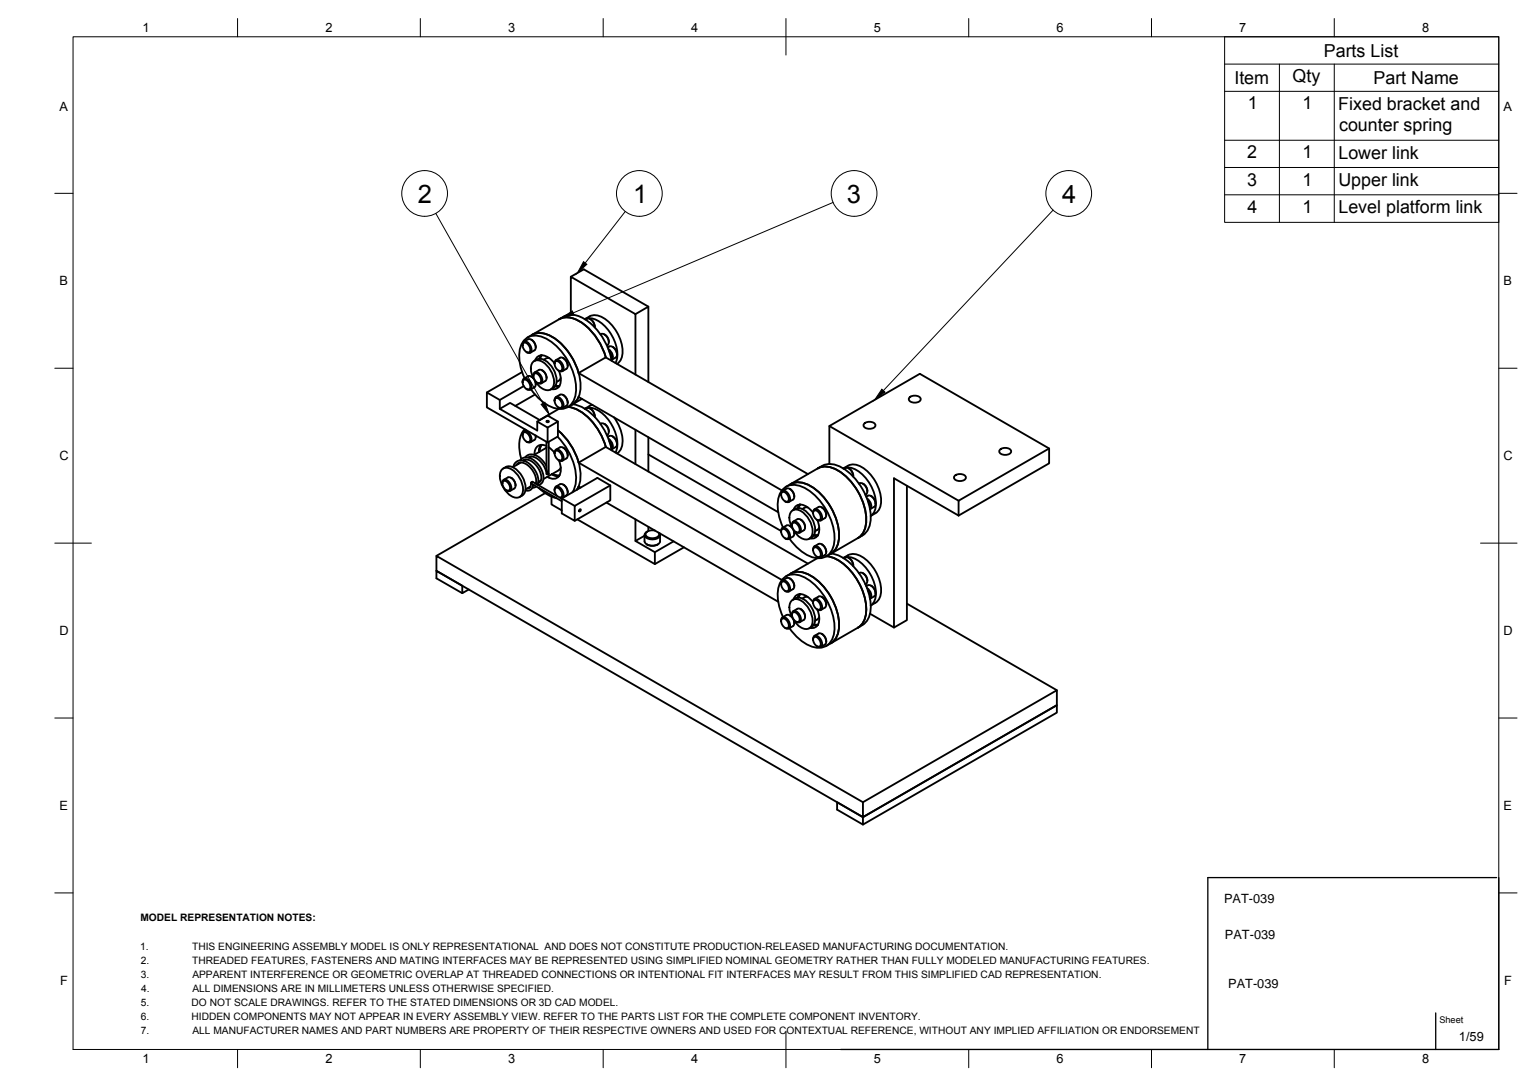
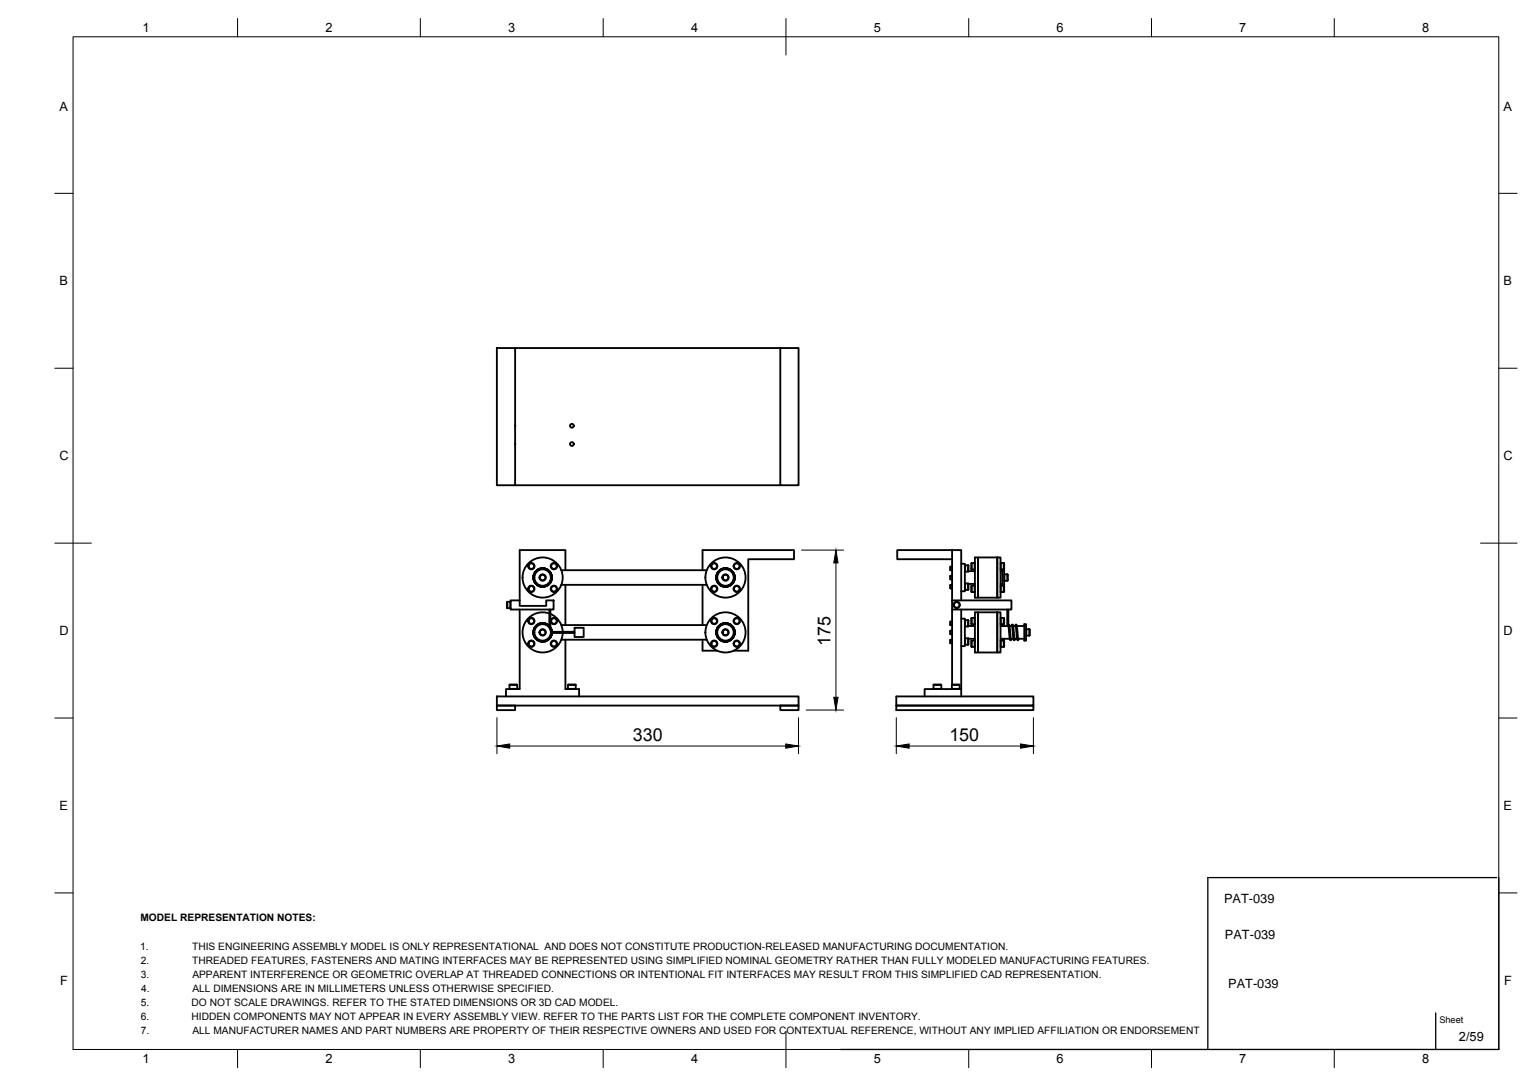
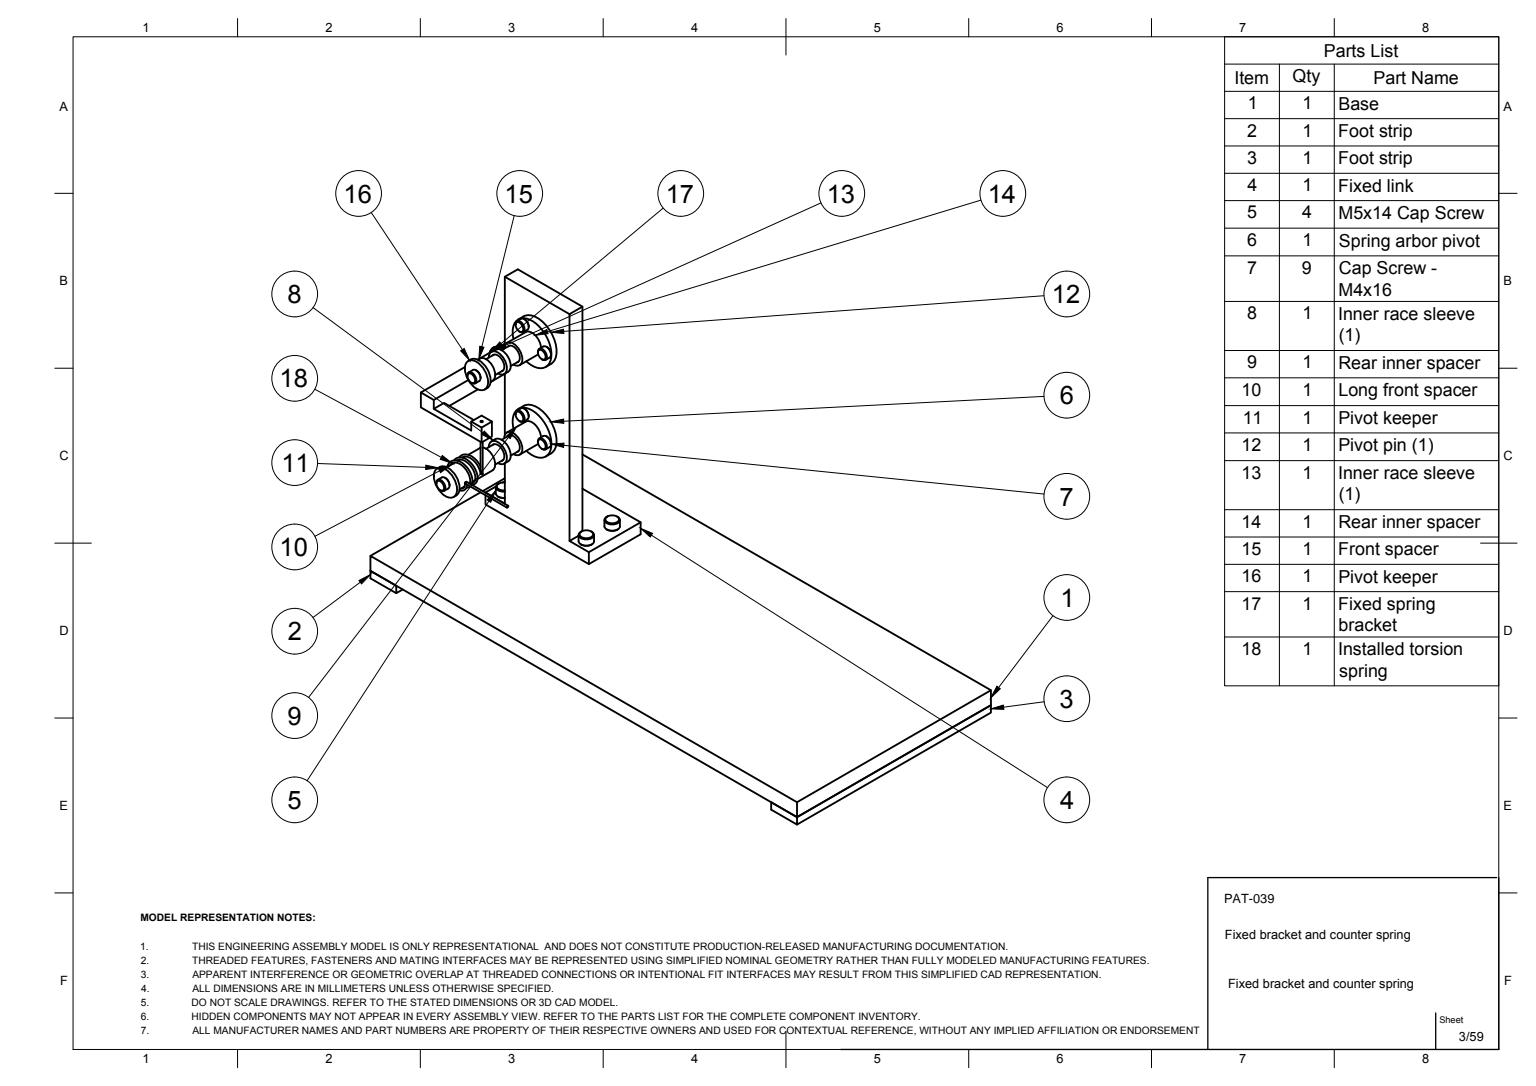
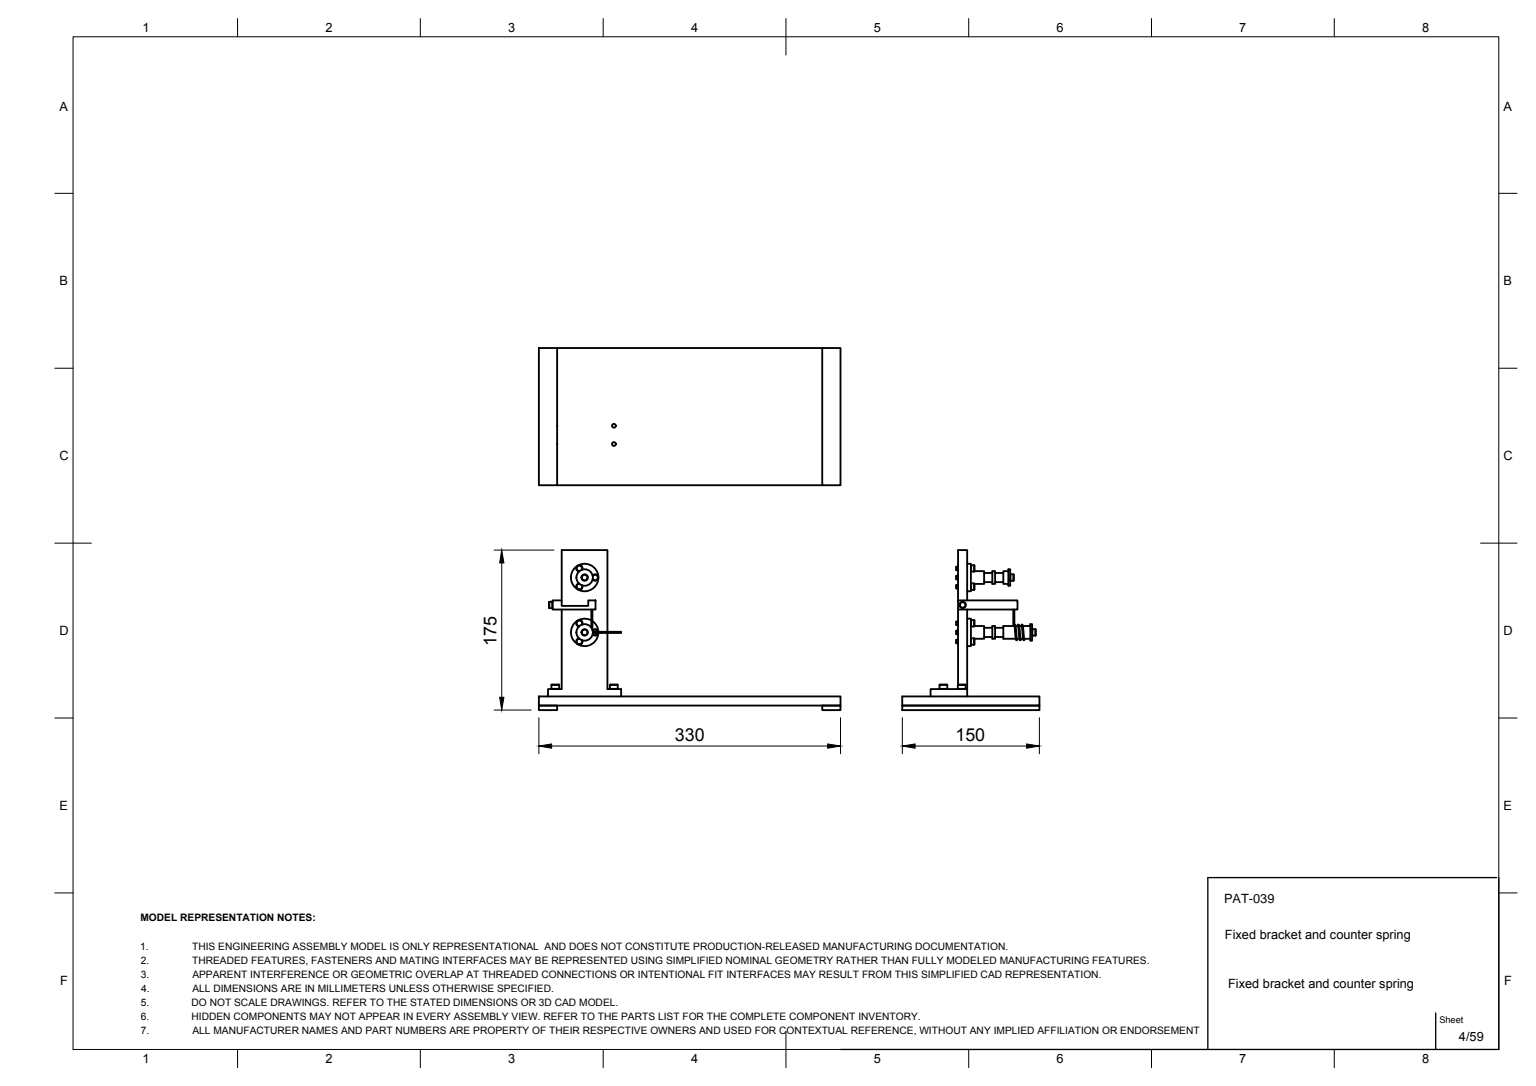
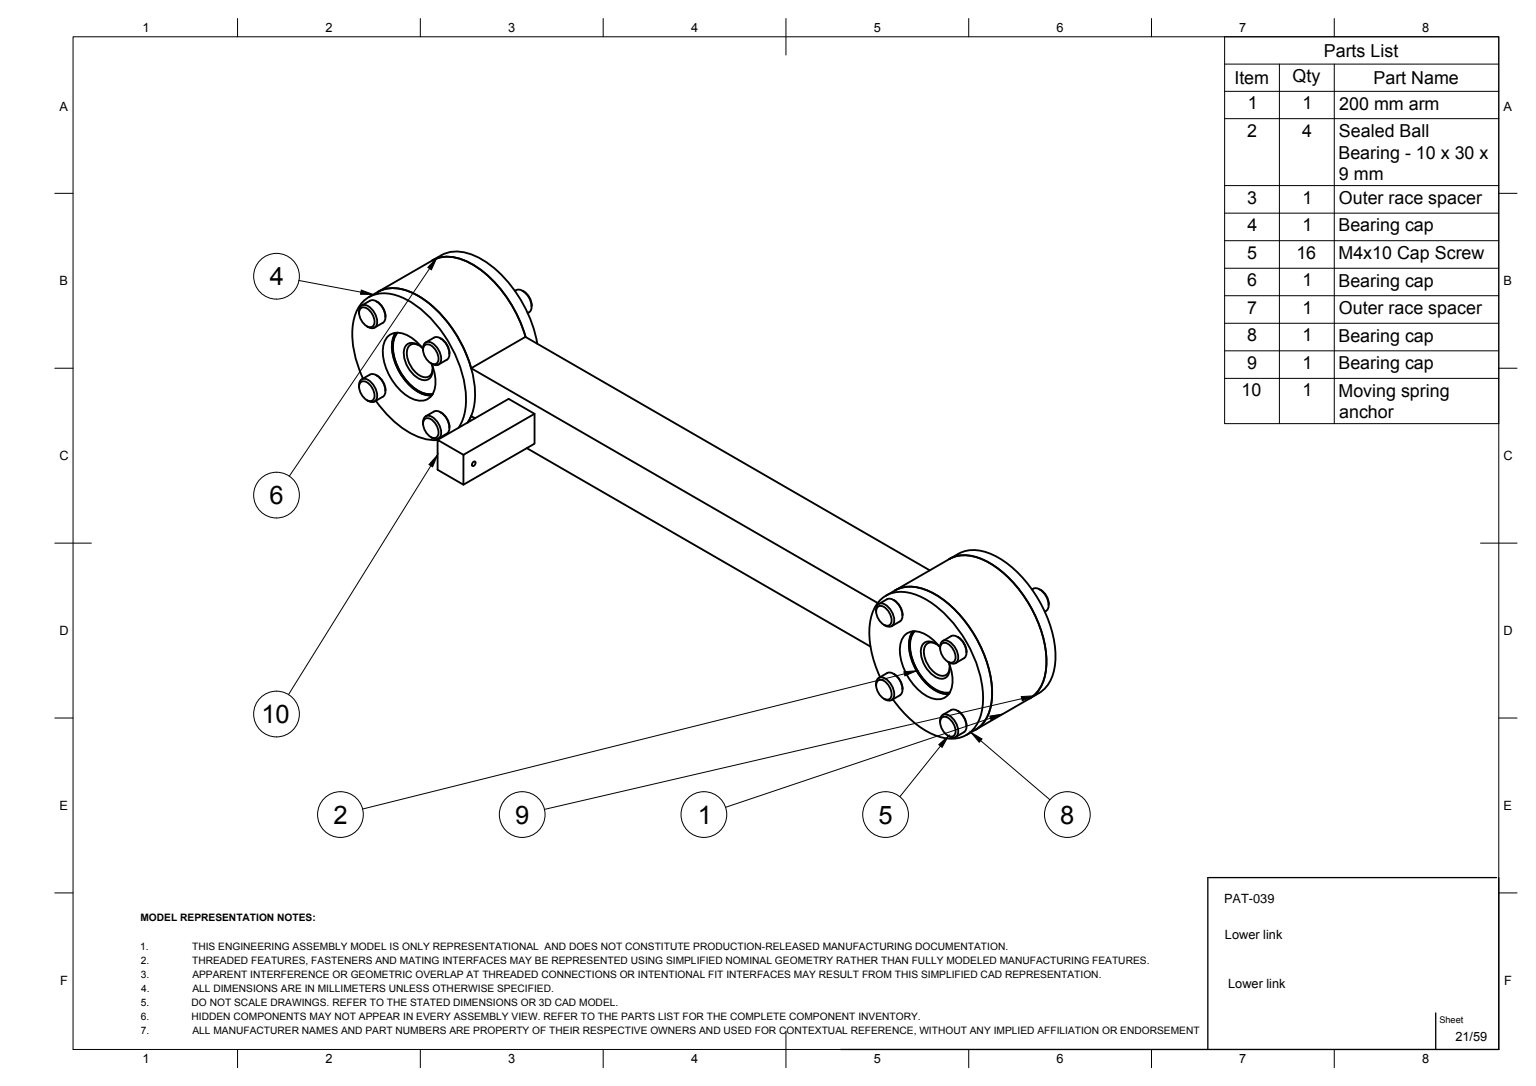
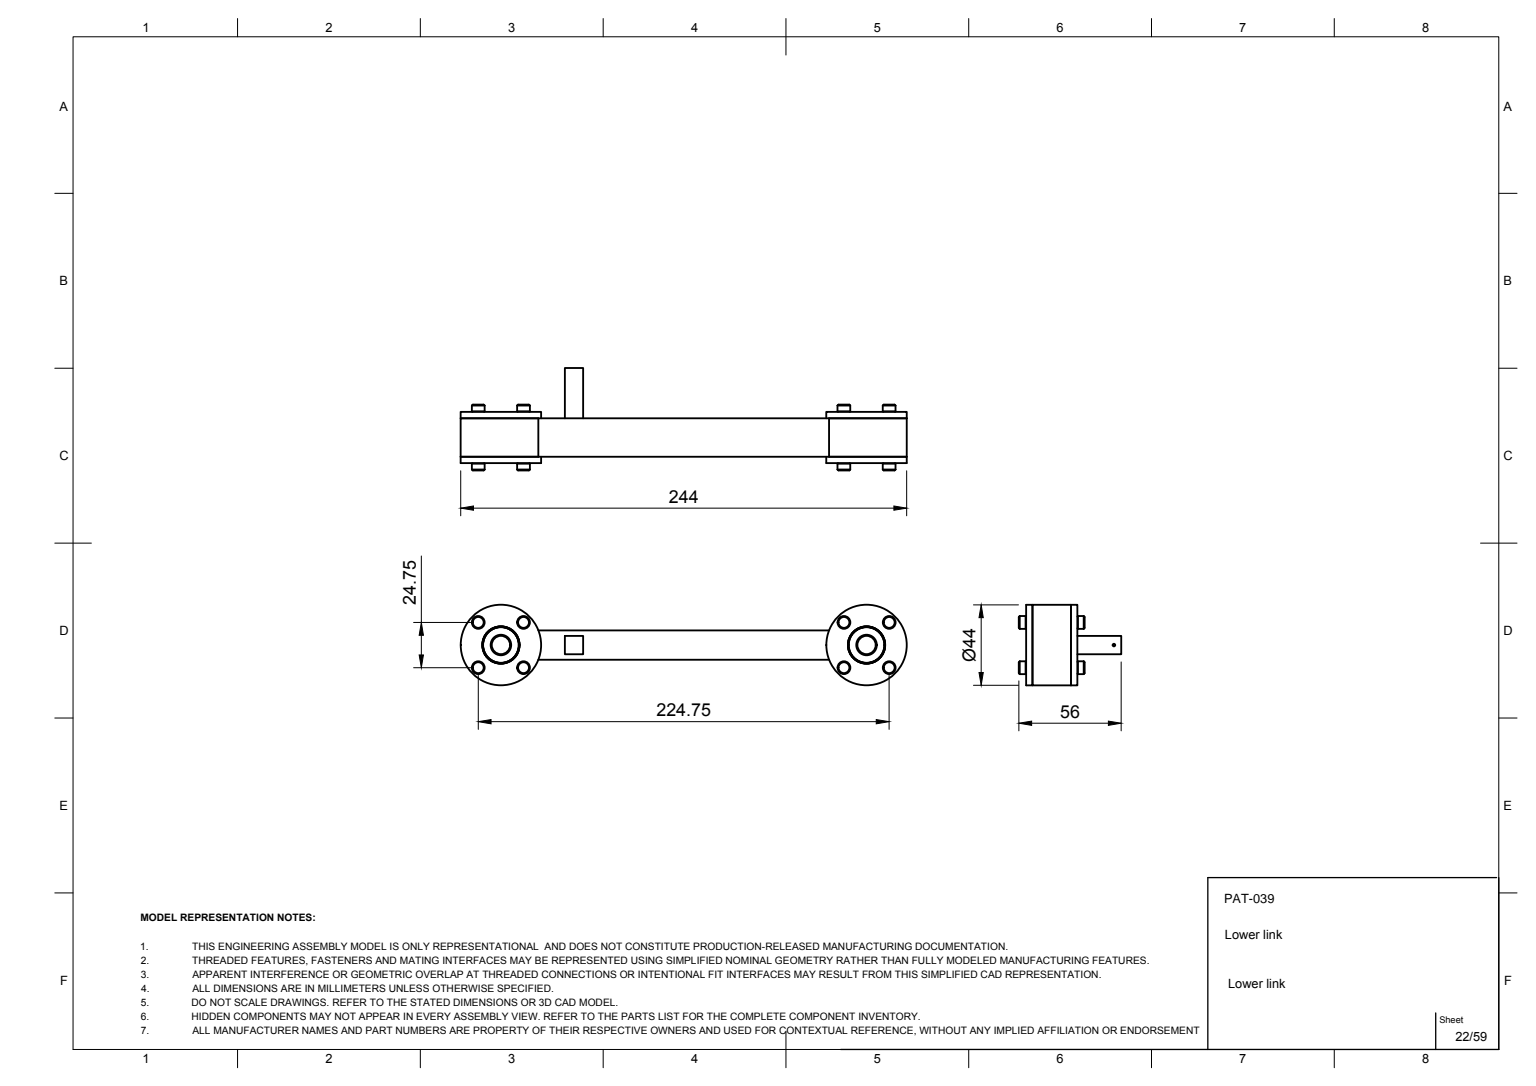
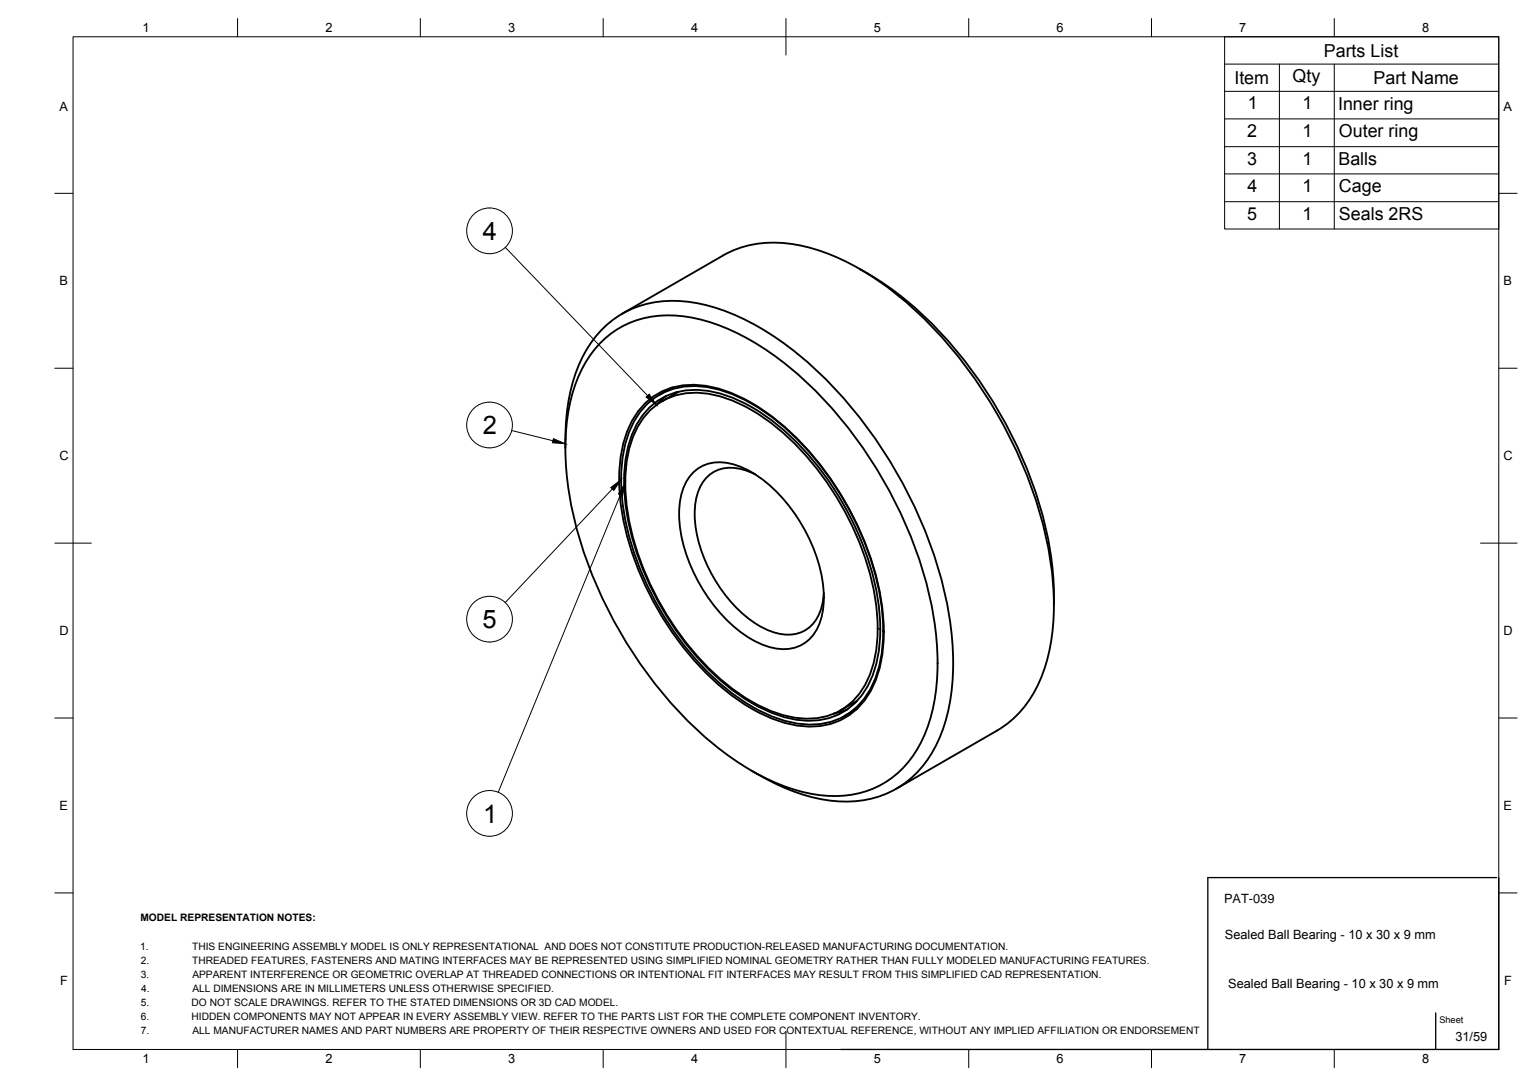
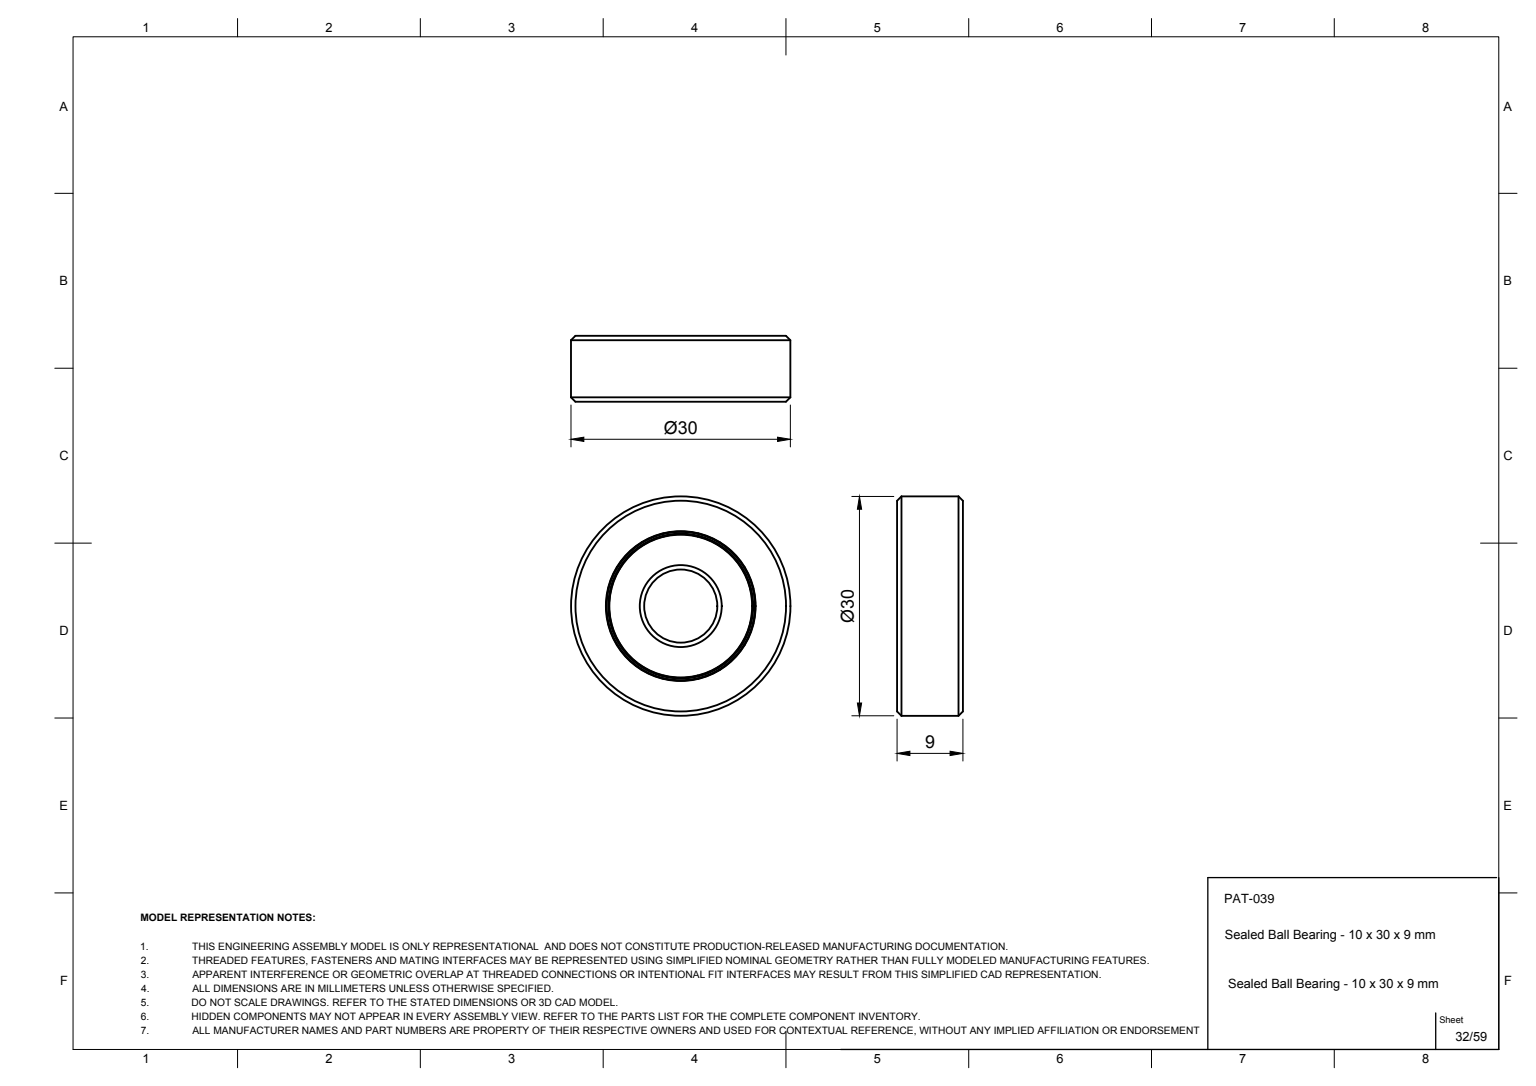
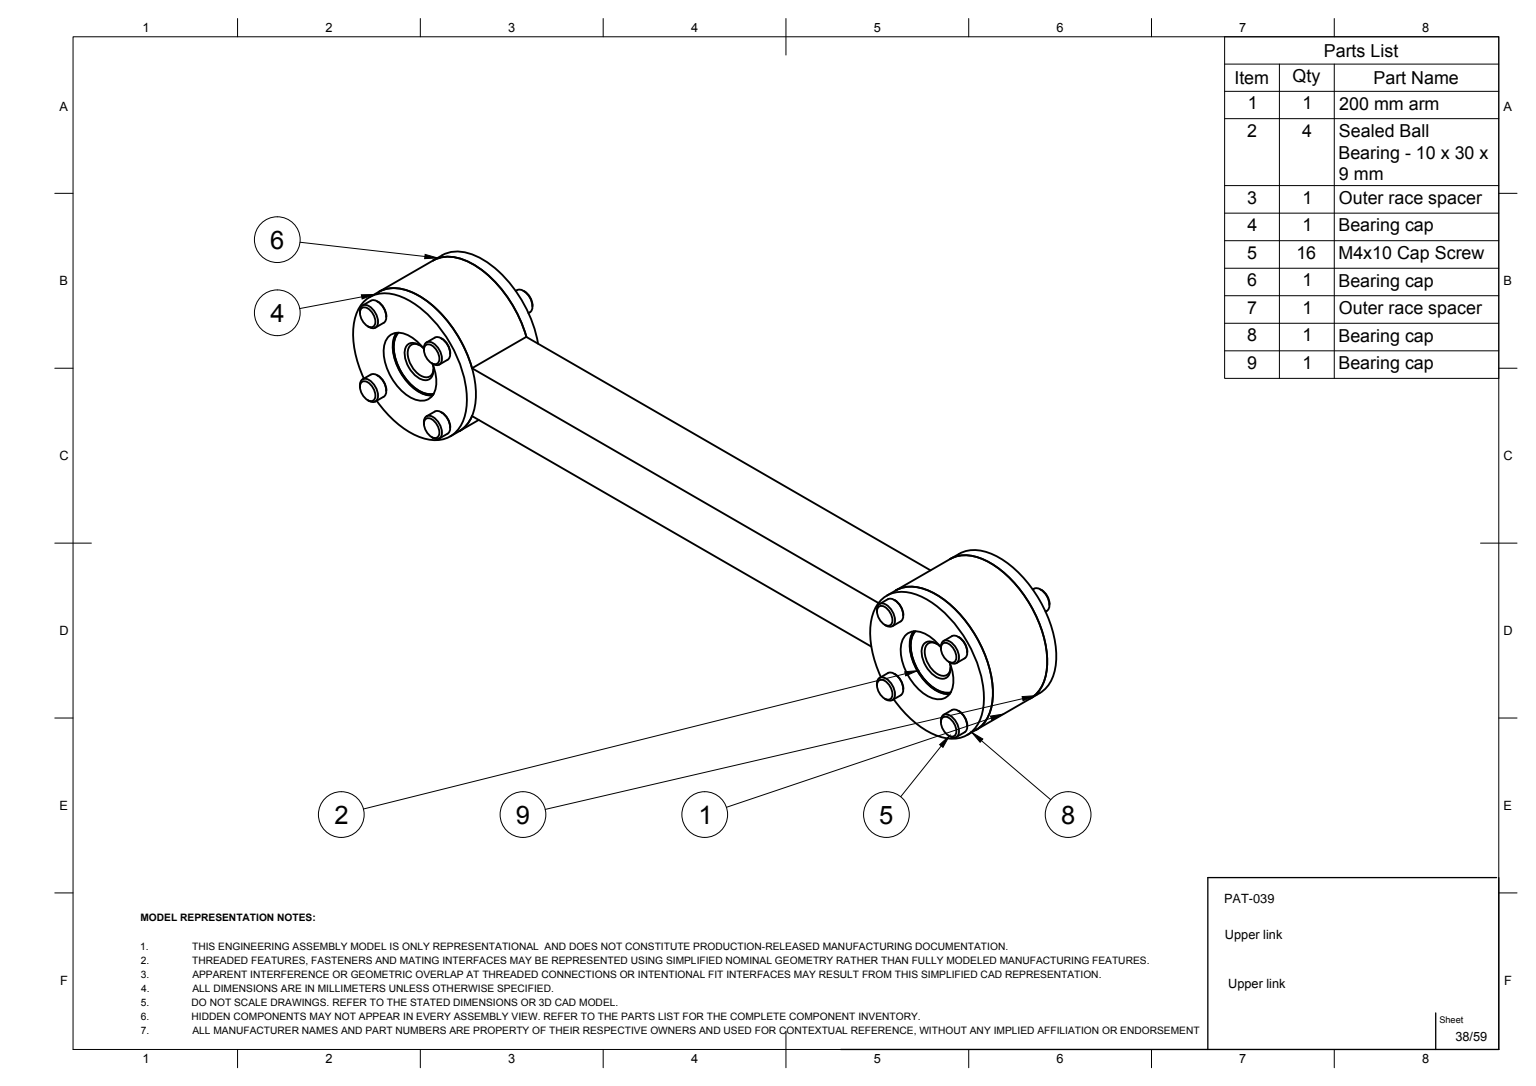
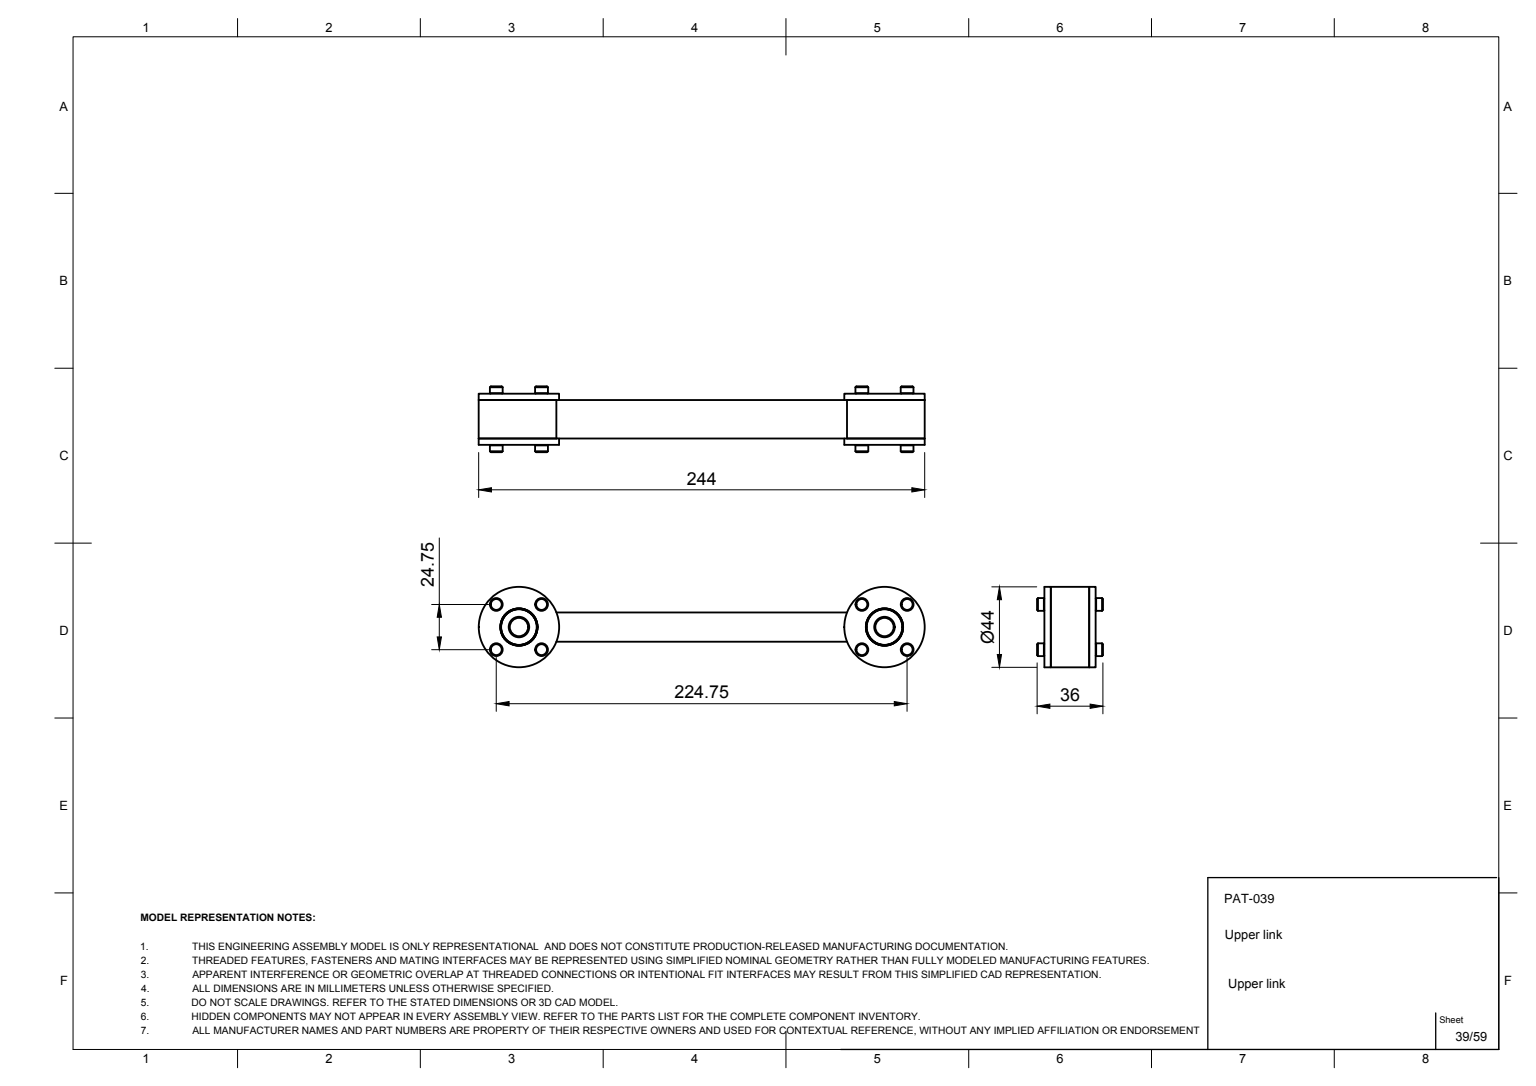
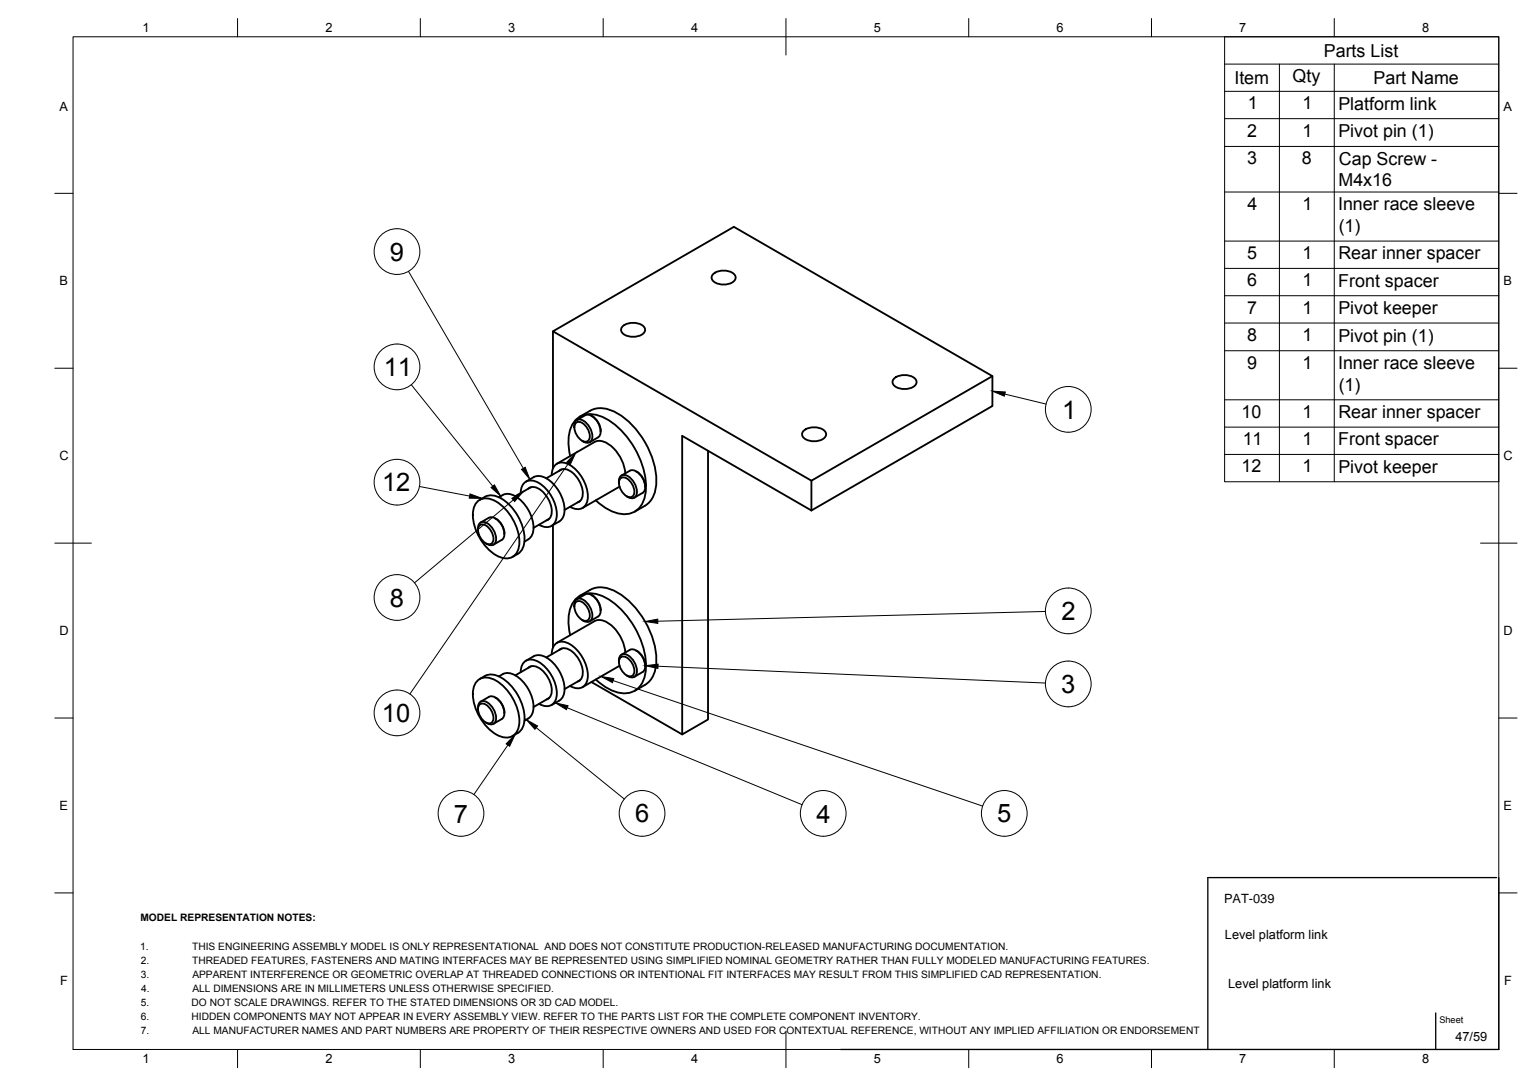
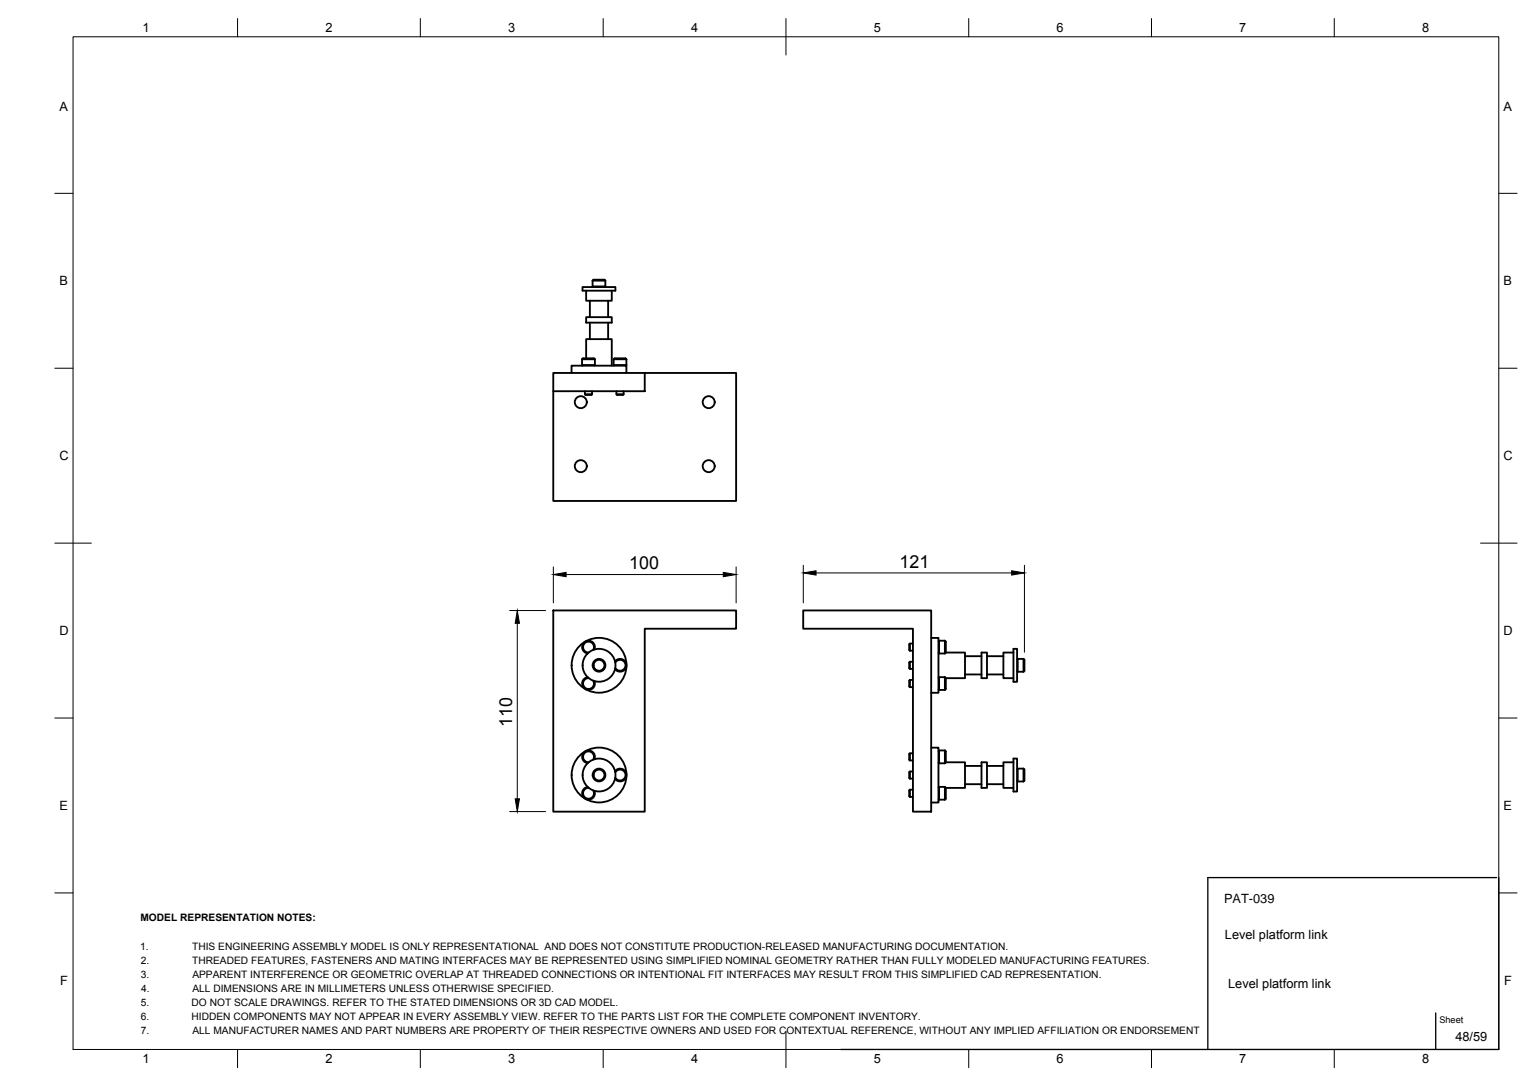
ISO-10303-21;
HEADER;
/* Generated by software containing ST-Developer
 * from STEP Tools, Inc. (www.steptools.com) 
 */

FILE_DESCRIPTION(
/* description */ ('Four-bar parallelogram arm'),
/* implementation_level */ '2;1');

FILE_NAME(
/* name */ 'PAT-039',
/* time_stamp */ '2026-10-28T03:24:55-07:00',
/* author */ (''),
/* organization */ (''),
/* preprocessor_version */ 'ST-DEVELOPER v20.2',
/* originating_system */ 'Autodesk Translation Framework v15.17.0.0',
/* authorisation */ '');

FILE_SCHEMA (('AUTOMOTIVE_DESIGN { 1 0 10303 214 3 1 1 }'));
ENDSEC;

DATA;
#10=MECHANICAL_DESIGN_GEOMETRIC_PRESENTATION_REPRESENTATION('',(#622,#623,
#624,#625,#626,#627,#628,#629,#630,#631,#632,#633,#634,#635,#636,#637,#638,
#639,#640,#641,#642,#643,#644,#645,#646,#647,#648,#649,#650,#651,#652,#653,
#654,#655,#656,#657,#658,#659,#660,#661,#662,#663,#664,#665,#666,#667,#668,
#669,#670,#671,#672,#673,#674,#675,#676,#677,#678,#679),#14512);
#11=ITEM_DEFINED_TRANSFORMATION($,$,#8507,#8635);
#12=ITEM_DEFINED_TRANSFORMATION($,$,#8527,#8636);
#13=ITEM_DEFINED_TRANSFORMATION($,$,#8547,#8637);
#14=ITEM_DEFINED_TRANSFORMATION($,$,#8564,#8638);
#15=ITEM_DEFINED_TRANSFORMATION($,$,#8618,#8639);
#16=ITEM_DEFINED_TRANSFORMATION($,$,#8209,#8664);
#17=ITEM_DEFINED_TRANSFORMATION($,$,#8250,#8665);
#18=ITEM_DEFINED_TRANSFORMATION($,$,#8259,#8666);
#19=ITEM_DEFINED_TRANSFORMATION($,$,#8280,#8667);
#20=ITEM_DEFINED_TRANSFORMATION($,$,#8301,#8668);
#21=ITEM_DEFINED_TRANSFORMATION($,$,#8310,#8669);
#22=ITEM_DEFINED_TRANSFORMATION($,$,#8331,#8670);
#23=ITEM_DEFINED_TRANSFORMATION($,$,#8352,#8671);
#24=ITEM_DEFINED_TRANSFORMATION($,$,#8506,#8672);
#25=ITEM_DEFINED_TRANSFORMATION($,$,#8506,#8673);
#26=ITEM_DEFINED_TRANSFORMATION($,$,#8640,#8674);
#27=ITEM_DEFINED_TRANSFORMATION($,$,#8640,#8675);
#28=ITEM_DEFINED_TRANSFORMATION($,$,#8640,#8676);
#29=ITEM_DEFINED_TRANSFORMATION($,$,#8640,#8677);
#30=ITEM_DEFINED_TRANSFORMATION($,$,#8640,#8678);
#31=ITEM_DEFINED_TRANSFORMATION($,$,#8640,#8679);
#32=ITEM_DEFINED_TRANSFORMATION($,$,#8640,#8680);
#33=ITEM_DEFINED_TRANSFORMATION($,$,#8640,#8681);
#34=ITEM_DEFINED_TRANSFORMATION($,$,#8506,#8682);
#35=ITEM_DEFINED_TRANSFORMATION($,$,#8506,#8683);
#36=ITEM_DEFINED_TRANSFORMATION($,$,#8640,#8684);
#37=ITEM_DEFINED_TRANSFORMATION($,$,#8640,#8685);
#38=ITEM_DEFINED_TRANSFORMATION($,$,#8640,#8686);
#39=ITEM_DEFINED_TRANSFORMATION($,$,#8640,#8687);
#40=ITEM_DEFINED_TRANSFORMATION($,$,#8640,#8688);
#41=ITEM_DEFINED_TRANSFORMATION($,$,#8640,#8689);
#42=ITEM_DEFINED_TRANSFORMATION($,$,#8640,#8690);
#43=ITEM_DEFINED_TRANSFORMATION($,$,#8640,#8691);
#44=ITEM_DEFINED_TRANSFORMATION($,$,#8363,#8692);
#45=ITEM_DEFINED_TRANSFORMATION($,$,#8404,#8693);
#46=ITEM_DEFINED_TRANSFORMATION($,$,#8413,#8694);
#47=ITEM_DEFINED_TRANSFORMATION($,$,#8434,#8695);
#48=ITEM_DEFINED_TRANSFORMATION($,$,#8455,#8696);
#49=ITEM_DEFINED_TRANSFORMATION($,$,#8464,#8697);
#50=ITEM_DEFINED_TRANSFORMATION($,$,#8485,#8698);
#51=ITEM_DEFINED_TRANSFORMATION($,$,#8506,#8699);
#52=ITEM_DEFINED_TRANSFORMATION($,$,#8506,#8700);
#53=ITEM_DEFINED_TRANSFORMATION($,$,#8640,#8701);
#54=ITEM_DEFINED_TRANSFORMATION($,$,#8640,#8702);
#55=ITEM_DEFINED_TRANSFORMATION($,$,#8640,#8703);
#56=ITEM_DEFINED_TRANSFORMATION($,$,#8640,#8704);
#57=ITEM_DEFINED_TRANSFORMATION($,$,#8640,#8705);
#58=ITEM_DEFINED_TRANSFORMATION($,$,#8640,#8706);
#59=ITEM_DEFINED_TRANSFORMATION($,$,#8640,#8707);
#60=ITEM_DEFINED_TRANSFORMATION($,$,#8640,#8708);
#61=ITEM_DEFINED_TRANSFORMATION($,$,#8506,#8709);
#62=ITEM_DEFINED_TRANSFORMATION($,$,#8506,#8710);
#63=ITEM_DEFINED_TRANSFORMATION($,$,#8640,#8711);
#64=ITEM_DEFINED_TRANSFORMATION($,$,#8640,#8712);
#65=ITEM_DEFINED_TRANSFORMATION($,$,#8640,#8713);
#66=ITEM_DEFINED_TRANSFORMATION($,$,#8640,#8714);
#67=ITEM_DEFINED_TRANSFORMATION($,$,#8640,#8715);
#68=ITEM_DEFINED_TRANSFORMATION($,$,#8640,#8716);
#69=ITEM_DEFINED_TRANSFORMATION($,$,#8640,#8717);
#70=ITEM_DEFINED_TRANSFORMATION($,$,#8640,#8718);
#71=ITEM_DEFINED_TRANSFORMATION($,$,#7940,#8918);
#72=ITEM_DEFINED_TRANSFORMATION($,$,#7959,#8919);
#73=ITEM_DEFINED_TRANSFORMATION($,$,#7966,#8920);
#74=ITEM_DEFINED_TRANSFORMATION($,$,#7973,#8921);
#75=ITEM_DEFINED_TRANSFORMATION($,$,#8024,#8922);
#76=ITEM_DEFINED_TRANSFORMATION($,$,#8051,#8923);
#77=ITEM_DEFINED_TRANSFORMATION($,$,#8060,#8924);
#78=ITEM_DEFINED_TRANSFORMATION($,$,#8069,#8925);
#79=ITEM_DEFINED_TRANSFORMATION($,$,#8078,#8926);
#80=ITEM_DEFINED_TRANSFORMATION($,$,#8087,#8927);
#81=ITEM_DEFINED_TRANSFORMATION($,$,#8114,#8928);
#82=ITEM_DEFINED_TRANSFORMATION($,$,#8123,#8929);
#83=ITEM_DEFINED_TRANSFORMATION($,$,#8132,#8930);
#84=ITEM_DEFINED_TRANSFORMATION($,$,#8141,#8931);
#85=ITEM_DEFINED_TRANSFORMATION($,$,#8150,#8932);
#86=ITEM_DEFINED_TRANSFORMATION($,$,#8168,#8933);
#87=ITEM_DEFINED_TRANSFORMATION($,$,#8184,#8934);
#88=ITEM_DEFINED_TRANSFORMATION($,$,#8184,#8935);
#89=ITEM_DEFINED_TRANSFORMATION($,$,#8184,#8936);
#90=ITEM_DEFINED_TRANSFORMATION($,$,#8184,#8937);
#91=ITEM_DEFINED_TRANSFORMATION($,$,#8892,#8938);
#92=ITEM_DEFINED_TRANSFORMATION($,$,#8892,#8939);
#93=ITEM_DEFINED_TRANSFORMATION($,$,#8892,#8940);
#94=ITEM_DEFINED_TRANSFORMATION($,$,#8892,#8941);
#95=ITEM_DEFINED_TRANSFORMATION($,$,#8892,#8942);
#96=ITEM_DEFINED_TRANSFORMATION($,$,#8892,#8943);
#97=ITEM_DEFINED_TRANSFORMATION($,$,#8892,#8944);
#98=ITEM_DEFINED_TRANSFORMATION($,$,#8892,#8945);
#99=ITEM_DEFINED_TRANSFORMATION($,$,#8892,#8946);
#100=ITEM_DEFINED_TRANSFORMATION($,$,#8720,#8947);
#101=ITEM_DEFINED_TRANSFORMATION($,$,#8766,#8948);
#102=ITEM_DEFINED_TRANSFORMATION($,$,#8793,#8949);
#103=ITEM_DEFINED_TRANSFORMATION($,$,#8802,#8950);
#104=ITEM_DEFINED_TRANSFORMATION($,$,#8811,#8951);
#105=ITEM_DEFINED_TRANSFORMATION($,$,#8820,#8952);
#106=ITEM_DEFINED_TRANSFORMATION($,$,#8829,#8953);
#107=ITEM_DEFINED_TRANSFORMATION($,$,#8856,#8954);
#108=ITEM_DEFINED_TRANSFORMATION($,$,#8865,#8955);
#109=ITEM_DEFINED_TRANSFORMATION($,$,#8874,#8956);
#110=ITEM_DEFINED_TRANSFORMATION($,$,#8883,#8957);
#111=ITEM_DEFINED_TRANSFORMATION($,$,#8892,#8958);
#112=ITEM_DEFINED_TRANSFORMATION($,$,#8892,#8959);
#113=ITEM_DEFINED_TRANSFORMATION($,$,#8892,#8960);
#114=ITEM_DEFINED_TRANSFORMATION($,$,#8892,#8961);
#115=ITEM_DEFINED_TRANSFORMATION($,$,#8892,#8962);
#116=ITEM_DEFINED_TRANSFORMATION($,$,#8892,#8963);
#117=ITEM_DEFINED_TRANSFORMATION($,$,#8892,#8964);
#118=ITEM_DEFINED_TRANSFORMATION($,$,#8892,#8965);
#119=ITEM_DEFINED_TRANSFORMATION($,$,#7939,#8966);
#120=ITEM_DEFINED_TRANSFORMATION($,$,#8208,#8967);
#121=ITEM_DEFINED_TRANSFORMATION($,$,#8362,#8968);
#122=ITEM_DEFINED_TRANSFORMATION($,$,#8719,#8969);
#123=(
REPRESENTATION_RELATIONSHIP($,$,#14778,#14777)
REPRESENTATION_RELATIONSHIP_WITH_TRANSFORMATION(#11)
SHAPE_REPRESENTATION_RELATIONSHIP()
);
#124=(
REPRESENTATION_RELATIONSHIP($,$,#14779,#14777)
REPRESENTATION_RELATIONSHIP_WITH_TRANSFORMATION(#12)
SHAPE_REPRESENTATION_RELATIONSHIP()
);
#125=(
REPRESENTATION_RELATIONSHIP($,$,#14780,#14777)
REPRESENTATION_RELATIONSHIP_WITH_TRANSFORMATION(#13)
SHAPE_REPRESENTATION_RELATIONSHIP()
);
#126=(
REPRESENTATION_RELATIONSHIP($,$,#14781,#14777)
REPRESENTATION_RELATIONSHIP_WITH_TRANSFORMATION(#14)
SHAPE_REPRESENTATION_RELATIONSHIP()
);
#127=(
REPRESENTATION_RELATIONSHIP($,$,#14782,#14777)
REPRESENTATION_RELATIONSHIP_WITH_TRANSFORMATION(#15)
SHAPE_REPRESENTATION_RELATIONSHIP()
);
#128=(
REPRESENTATION_RELATIONSHIP($,$,#14761,#14760)
REPRESENTATION_RELATIONSHIP_WITH_TRANSFORMATION(#16)
SHAPE_REPRESENTATION_RELATIONSHIP()
);
#129=(
REPRESENTATION_RELATIONSHIP($,$,#14762,#14760)
REPRESENTATION_RELATIONSHIP_WITH_TRANSFORMATION(#17)
SHAPE_REPRESENTATION_RELATIONSHIP()
);
#130=(
REPRESENTATION_RELATIONSHIP($,$,#14763,#14760)
REPRESENTATION_RELATIONSHIP_WITH_TRANSFORMATION(#18)
SHAPE_REPRESENTATION_RELATIONSHIP()
);
#131=(
REPRESENTATION_RELATIONSHIP($,$,#14764,#14760)
REPRESENTATION_RELATIONSHIP_WITH_TRANSFORMATION(#19)
SHAPE_REPRESENTATION_RELATIONSHIP()
);
#132=(
REPRESENTATION_RELATIONSHIP($,$,#14765,#14760)
REPRESENTATION_RELATIONSHIP_WITH_TRANSFORMATION(#20)
SHAPE_REPRESENTATION_RELATIONSHIP()
);
#133=(
REPRESENTATION_RELATIONSHIP($,$,#14766,#14760)
REPRESENTATION_RELATIONSHIP_WITH_TRANSFORMATION(#21)
SHAPE_REPRESENTATION_RELATIONSHIP()
);
#134=(
REPRESENTATION_RELATIONSHIP($,$,#14767,#14760)
REPRESENTATION_RELATIONSHIP_WITH_TRANSFORMATION(#22)
SHAPE_REPRESENTATION_RELATIONSHIP()
);
#135=(
REPRESENTATION_RELATIONSHIP($,$,#14768,#14760)
REPRESENTATION_RELATIONSHIP_WITH_TRANSFORMATION(#23)
SHAPE_REPRESENTATION_RELATIONSHIP()
);
#136=(
REPRESENTATION_RELATIONSHIP($,$,#14777,#14760)
REPRESENTATION_RELATIONSHIP_WITH_TRANSFORMATION(#24)
SHAPE_REPRESENTATION_RELATIONSHIP()
);
#137=(
REPRESENTATION_RELATIONSHIP($,$,#14777,#14760)
REPRESENTATION_RELATIONSHIP_WITH_TRANSFORMATION(#25)
SHAPE_REPRESENTATION_RELATIONSHIP()
);
#138=(
REPRESENTATION_RELATIONSHIP($,$,#14783,#14760)
REPRESENTATION_RELATIONSHIP_WITH_TRANSFORMATION(#26)
SHAPE_REPRESENTATION_RELATIONSHIP()
);
#139=(
REPRESENTATION_RELATIONSHIP($,$,#14783,#14760)
REPRESENTATION_RELATIONSHIP_WITH_TRANSFORMATION(#27)
SHAPE_REPRESENTATION_RELATIONSHIP()
);
#140=(
REPRESENTATION_RELATIONSHIP($,$,#14783,#14760)
REPRESENTATION_RELATIONSHIP_WITH_TRANSFORMATION(#28)
SHAPE_REPRESENTATION_RELATIONSHIP()
);
#141=(
REPRESENTATION_RELATIONSHIP($,$,#14783,#14760)
REPRESENTATION_RELATIONSHIP_WITH_TRANSFORMATION(#29)
SHAPE_REPRESENTATION_RELATIONSHIP()
);
#142=(
REPRESENTATION_RELATIONSHIP($,$,#14783,#14760)
REPRESENTATION_RELATIONSHIP_WITH_TRANSFORMATION(#30)
SHAPE_REPRESENTATION_RELATIONSHIP()
);
#143=(
REPRESENTATION_RELATIONSHIP($,$,#14783,#14760)
REPRESENTATION_RELATIONSHIP_WITH_TRANSFORMATION(#31)
SHAPE_REPRESENTATION_RELATIONSHIP()
);
#144=(
REPRESENTATION_RELATIONSHIP($,$,#14783,#14760)
REPRESENTATION_RELATIONSHIP_WITH_TRANSFORMATION(#32)
SHAPE_REPRESENTATION_RELATIONSHIP()
);
#145=(
REPRESENTATION_RELATIONSHIP($,$,#14783,#14760)
REPRESENTATION_RELATIONSHIP_WITH_TRANSFORMATION(#33)
SHAPE_REPRESENTATION_RELATIONSHIP()
);
#146=(
REPRESENTATION_RELATIONSHIP($,$,#14777,#14760)
REPRESENTATION_RELATIONSHIP_WITH_TRANSFORMATION(#34)
SHAPE_REPRESENTATION_RELATIONSHIP()
);
#147=(
REPRESENTATION_RELATIONSHIP($,$,#14777,#14760)
REPRESENTATION_RELATIONSHIP_WITH_TRANSFORMATION(#35)
SHAPE_REPRESENTATION_RELATIONSHIP()
);
#148=(
REPRESENTATION_RELATIONSHIP($,$,#14783,#14760)
REPRESENTATION_RELATIONSHIP_WITH_TRANSFORMATION(#36)
SHAPE_REPRESENTATION_RELATIONSHIP()
);
#149=(
REPRESENTATION_RELATIONSHIP($,$,#14783,#14760)
REPRESENTATION_RELATIONSHIP_WITH_TRANSFORMATION(#37)
SHAPE_REPRESENTATION_RELATIONSHIP()
);
#150=(
REPRESENTATION_RELATIONSHIP($,$,#14783,#14760)
REPRESENTATION_RELATIONSHIP_WITH_TRANSFORMATION(#38)
SHAPE_REPRESENTATION_RELATIONSHIP()
);
#151=(
REPRESENTATION_RELATIONSHIP($,$,#14783,#14760)
REPRESENTATION_RELATIONSHIP_WITH_TRANSFORMATION(#39)
SHAPE_REPRESENTATION_RELATIONSHIP()
);
#152=(
REPRESENTATION_RELATIONSHIP($,$,#14783,#14760)
REPRESENTATION_RELATIONSHIP_WITH_TRANSFORMATION(#40)
SHAPE_REPRESENTATION_RELATIONSHIP()
);
#153=(
REPRESENTATION_RELATIONSHIP($,$,#14783,#14760)
REPRESENTATION_RELATIONSHIP_WITH_TRANSFORMATION(#41)
SHAPE_REPRESENTATION_RELATIONSHIP()
);
#154=(
REPRESENTATION_RELATIONSHIP($,$,#14783,#14760)
REPRESENTATION_RELATIONSHIP_WITH_TRANSFORMATION(#42)
SHAPE_REPRESENTATION_RELATIONSHIP()
);
#155=(
REPRESENTATION_RELATIONSHIP($,$,#14783,#14760)
REPRESENTATION_RELATIONSHIP_WITH_TRANSFORMATION(#43)
SHAPE_REPRESENTATION_RELATIONSHIP()
);
#156=(
REPRESENTATION_RELATIONSHIP($,$,#14770,#14769)
REPRESENTATION_RELATIONSHIP_WITH_TRANSFORMATION(#44)
SHAPE_REPRESENTATION_RELATIONSHIP()
);
#157=(
REPRESENTATION_RELATIONSHIP($,$,#14771,#14769)
REPRESENTATION_RELATIONSHIP_WITH_TRANSFORMATION(#45)
SHAPE_REPRESENTATION_RELATIONSHIP()
);
#158=(
REPRESENTATION_RELATIONSHIP($,$,#14772,#14769)
REPRESENTATION_RELATIONSHIP_WITH_TRANSFORMATION(#46)
SHAPE_REPRESENTATION_RELATIONSHIP()
);
#159=(
REPRESENTATION_RELATIONSHIP($,$,#14773,#14769)
REPRESENTATION_RELATIONSHIP_WITH_TRANSFORMATION(#47)
SHAPE_REPRESENTATION_RELATIONSHIP()
);
#160=(
REPRESENTATION_RELATIONSHIP($,$,#14774,#14769)
REPRESENTATION_RELATIONSHIP_WITH_TRANSFORMATION(#48)
SHAPE_REPRESENTATION_RELATIONSHIP()
);
#161=(
REPRESENTATION_RELATIONSHIP($,$,#14775,#14769)
REPRESENTATION_RELATIONSHIP_WITH_TRANSFORMATION(#49)
SHAPE_REPRESENTATION_RELATIONSHIP()
);
#162=(
REPRESENTATION_RELATIONSHIP($,$,#14776,#14769)
REPRESENTATION_RELATIONSHIP_WITH_TRANSFORMATION(#50)
SHAPE_REPRESENTATION_RELATIONSHIP()
);
#163=(
REPRESENTATION_RELATIONSHIP($,$,#14777,#14769)
REPRESENTATION_RELATIONSHIP_WITH_TRANSFORMATION(#51)
SHAPE_REPRESENTATION_RELATIONSHIP()
);
#164=(
REPRESENTATION_RELATIONSHIP($,$,#14777,#14769)
REPRESENTATION_RELATIONSHIP_WITH_TRANSFORMATION(#52)
SHAPE_REPRESENTATION_RELATIONSHIP()
);
#165=(
REPRESENTATION_RELATIONSHIP($,$,#14783,#14769)
REPRESENTATION_RELATIONSHIP_WITH_TRANSFORMATION(#53)
SHAPE_REPRESENTATION_RELATIONSHIP()
);
#166=(
REPRESENTATION_RELATIONSHIP($,$,#14783,#14769)
REPRESENTATION_RELATIONSHIP_WITH_TRANSFORMATION(#54)
SHAPE_REPRESENTATION_RELATIONSHIP()
);
#167=(
REPRESENTATION_RELATIONSHIP($,$,#14783,#14769)
REPRESENTATION_RELATIONSHIP_WITH_TRANSFORMATION(#55)
SHAPE_REPRESENTATION_RELATIONSHIP()
);
#168=(
REPRESENTATION_RELATIONSHIP($,$,#14783,#14769)
REPRESENTATION_RELATIONSHIP_WITH_TRANSFORMATION(#56)
SHAPE_REPRESENTATION_RELATIONSHIP()
);
#169=(
REPRESENTATION_RELATIONSHIP($,$,#14783,#14769)
REPRESENTATION_RELATIONSHIP_WITH_TRANSFORMATION(#57)
SHAPE_REPRESENTATION_RELATIONSHIP()
);
#170=(
REPRESENTATION_RELATIONSHIP($,$,#14783,#14769)
REPRESENTATION_RELATIONSHIP_WITH_TRANSFORMATION(#58)
SHAPE_REPRESENTATION_RELATIONSHIP()
);
#171=(
REPRESENTATION_RELATIONSHIP($,$,#14783,#14769)
REPRESENTATION_RELATIONSHIP_WITH_TRANSFORMATION(#59)
SHAPE_REPRESENTATION_RELATIONSHIP()
);
#172=(
REPRESENTATION_RELATIONSHIP($,$,#14783,#14769)
REPRESENTATION_RELATIONSHIP_WITH_TRANSFORMATION(#60)
SHAPE_REPRESENTATION_RELATIONSHIP()
);
#173=(
REPRESENTATION_RELATIONSHIP($,$,#14777,#14769)
REPRESENTATION_RELATIONSHIP_WITH_TRANSFORMATION(#61)
SHAPE_REPRESENTATION_RELATIONSHIP()
);
#174=(
REPRESENTATION_RELATIONSHIP($,$,#14777,#14769)
REPRESENTATION_RELATIONSHIP_WITH_TRANSFORMATION(#62)
SHAPE_REPRESENTATION_RELATIONSHIP()
);
#175=(
REPRESENTATION_RELATIONSHIP($,$,#14783,#14769)
REPRESENTATION_RELATIONSHIP_WITH_TRANSFORMATION(#63)
SHAPE_REPRESENTATION_RELATIONSHIP()
);
#176=(
REPRESENTATION_RELATIONSHIP($,$,#14783,#14769)
REPRESENTATION_RELATIONSHIP_WITH_TRANSFORMATION(#64)
SHAPE_REPRESENTATION_RELATIONSHIP()
);
#177=(
REPRESENTATION_RELATIONSHIP($,$,#14783,#14769)
REPRESENTATION_RELATIONSHIP_WITH_TRANSFORMATION(#65)
SHAPE_REPRESENTATION_RELATIONSHIP()
);
#178=(
REPRESENTATION_RELATIONSHIP($,$,#14783,#14769)
REPRESENTATION_RELATIONSHIP_WITH_TRANSFORMATION(#66)
SHAPE_REPRESENTATION_RELATIONSHIP()
);
#179=(
REPRESENTATION_RELATIONSHIP($,$,#14783,#14769)
REPRESENTATION_RELATIONSHIP_WITH_TRANSFORMATION(#67)
SHAPE_REPRESENTATION_RELATIONSHIP()
);
#180=(
REPRESENTATION_RELATIONSHIP($,$,#14783,#14769)
REPRESENTATION_RELATIONSHIP_WITH_TRANSFORMATION(#68)
SHAPE_REPRESENTATION_RELATIONSHIP()
);
#181=(
REPRESENTATION_RELATIONSHIP($,$,#14783,#14769)
REPRESENTATION_RELATIONSHIP_WITH_TRANSFORMATION(#69)
SHAPE_REPRESENTATION_RELATIONSHIP()
);
#182=(
REPRESENTATION_RELATIONSHIP($,$,#14783,#14769)
REPRESENTATION_RELATIONSHIP_WITH_TRANSFORMATION(#70)
SHAPE_REPRESENTATION_RELATIONSHIP()
);
#183=(
REPRESENTATION_RELATIONSHIP($,$,#14743,#14742)
REPRESENTATION_RELATIONSHIP_WITH_TRANSFORMATION(#71)
SHAPE_REPRESENTATION_RELATIONSHIP()
);
#184=(
REPRESENTATION_RELATIONSHIP($,$,#14744,#14742)
REPRESENTATION_RELATIONSHIP_WITH_TRANSFORMATION(#72)
SHAPE_REPRESENTATION_RELATIONSHIP()
);
#185=(
REPRESENTATION_RELATIONSHIP($,$,#14745,#14742)
REPRESENTATION_RELATIONSHIP_WITH_TRANSFORMATION(#73)
SHAPE_REPRESENTATION_RELATIONSHIP()
);
#186=(
REPRESENTATION_RELATIONSHIP($,$,#14746,#14742)
REPRESENTATION_RELATIONSHIP_WITH_TRANSFORMATION(#74)
SHAPE_REPRESENTATION_RELATIONSHIP()
);
#187=(
REPRESENTATION_RELATIONSHIP($,$,#14747,#14742)
REPRESENTATION_RELATIONSHIP_WITH_TRANSFORMATION(#75)
SHAPE_REPRESENTATION_RELATIONSHIP()
);
#188=(
REPRESENTATION_RELATIONSHIP($,$,#14748,#14742)
REPRESENTATION_RELATIONSHIP_WITH_TRANSFORMATION(#76)
SHAPE_REPRESENTATION_RELATIONSHIP()
);
#189=(
REPRESENTATION_RELATIONSHIP($,$,#14749,#14742)
REPRESENTATION_RELATIONSHIP_WITH_TRANSFORMATION(#77)
SHAPE_REPRESENTATION_RELATIONSHIP()
);
#190=(
REPRESENTATION_RELATIONSHIP($,$,#14750,#14742)
REPRESENTATION_RELATIONSHIP_WITH_TRANSFORMATION(#78)
SHAPE_REPRESENTATION_RELATIONSHIP()
);
#191=(
REPRESENTATION_RELATIONSHIP($,$,#14751,#14742)
REPRESENTATION_RELATIONSHIP_WITH_TRANSFORMATION(#79)
SHAPE_REPRESENTATION_RELATIONSHIP()
);
#192=(
REPRESENTATION_RELATIONSHIP($,$,#14752,#14742)
REPRESENTATION_RELATIONSHIP_WITH_TRANSFORMATION(#80)
SHAPE_REPRESENTATION_RELATIONSHIP()
);
#193=(
REPRESENTATION_RELATIONSHIP($,$,#14753,#14742)
REPRESENTATION_RELATIONSHIP_WITH_TRANSFORMATION(#81)
SHAPE_REPRESENTATION_RELATIONSHIP()
);
#194=(
REPRESENTATION_RELATIONSHIP($,$,#14754,#14742)
REPRESENTATION_RELATIONSHIP_WITH_TRANSFORMATION(#82)
SHAPE_REPRESENTATION_RELATIONSHIP()
);
#195=(
REPRESENTATION_RELATIONSHIP($,$,#14755,#14742)
REPRESENTATION_RELATIONSHIP_WITH_TRANSFORMATION(#83)
SHAPE_REPRESENTATION_RELATIONSHIP()
);
#196=(
REPRESENTATION_RELATIONSHIP($,$,#14756,#14742)
REPRESENTATION_RELATIONSHIP_WITH_TRANSFORMATION(#84)
SHAPE_REPRESENTATION_RELATIONSHIP()
);
#197=(
REPRESENTATION_RELATIONSHIP($,$,#14757,#14742)
REPRESENTATION_RELATIONSHIP_WITH_TRANSFORMATION(#85)
SHAPE_REPRESENTATION_RELATIONSHIP()
);
#198=(
REPRESENTATION_RELATIONSHIP($,$,#14758,#14742)
REPRESENTATION_RELATIONSHIP_WITH_TRANSFORMATION(#86)
SHAPE_REPRESENTATION_RELATIONSHIP()
);
#199=(
REPRESENTATION_RELATIONSHIP($,$,#14759,#14742)
REPRESENTATION_RELATIONSHIP_WITH_TRANSFORMATION(#87)
SHAPE_REPRESENTATION_RELATIONSHIP()
);
#200=(
REPRESENTATION_RELATIONSHIP($,$,#14759,#14742)
REPRESENTATION_RELATIONSHIP_WITH_TRANSFORMATION(#88)
SHAPE_REPRESENTATION_RELATIONSHIP()
);
#201=(
REPRESENTATION_RELATIONSHIP($,$,#14759,#14742)
REPRESENTATION_RELATIONSHIP_WITH_TRANSFORMATION(#89)
SHAPE_REPRESENTATION_RELATIONSHIP()
);
#202=(
REPRESENTATION_RELATIONSHIP($,$,#14759,#14742)
REPRESENTATION_RELATIONSHIP_WITH_TRANSFORMATION(#90)
SHAPE_REPRESENTATION_RELATIONSHIP()
);
#203=(
REPRESENTATION_RELATIONSHIP($,$,#14796,#14742)
REPRESENTATION_RELATIONSHIP_WITH_TRANSFORMATION(#91)
SHAPE_REPRESENTATION_RELATIONSHIP()
);
#204=(
REPRESENTATION_RELATIONSHIP($,$,#14796,#14742)
REPRESENTATION_RELATIONSHIP_WITH_TRANSFORMATION(#92)
SHAPE_REPRESENTATION_RELATIONSHIP()
);
#205=(
REPRESENTATION_RELATIONSHIP($,$,#14796,#14742)
REPRESENTATION_RELATIONSHIP_WITH_TRANSFORMATION(#93)
SHAPE_REPRESENTATION_RELATIONSHIP()
);
#206=(
REPRESENTATION_RELATIONSHIP($,$,#14796,#14742)
REPRESENTATION_RELATIONSHIP_WITH_TRANSFORMATION(#94)
SHAPE_REPRESENTATION_RELATIONSHIP()
);
#207=(
REPRESENTATION_RELATIONSHIP($,$,#14796,#14742)
REPRESENTATION_RELATIONSHIP_WITH_TRANSFORMATION(#95)
SHAPE_REPRESENTATION_RELATIONSHIP()
);
#208=(
REPRESENTATION_RELATIONSHIP($,$,#14796,#14742)
REPRESENTATION_RELATIONSHIP_WITH_TRANSFORMATION(#96)
SHAPE_REPRESENTATION_RELATIONSHIP()
);
#209=(
REPRESENTATION_RELATIONSHIP($,$,#14796,#14742)
REPRESENTATION_RELATIONSHIP_WITH_TRANSFORMATION(#97)
SHAPE_REPRESENTATION_RELATIONSHIP()
);
#210=(
REPRESENTATION_RELATIONSHIP($,$,#14796,#14742)
REPRESENTATION_RELATIONSHIP_WITH_TRANSFORMATION(#98)
SHAPE_REPRESENTATION_RELATIONSHIP()
);
#211=(
REPRESENTATION_RELATIONSHIP($,$,#14796,#14742)
REPRESENTATION_RELATIONSHIP_WITH_TRANSFORMATION(#99)
SHAPE_REPRESENTATION_RELATIONSHIP()
);
#212=(
REPRESENTATION_RELATIONSHIP($,$,#14785,#14784)
REPRESENTATION_RELATIONSHIP_WITH_TRANSFORMATION(#100)
SHAPE_REPRESENTATION_RELATIONSHIP()
);
#213=(
REPRESENTATION_RELATIONSHIP($,$,#14786,#14784)
REPRESENTATION_RELATIONSHIP_WITH_TRANSFORMATION(#101)
SHAPE_REPRESENTATION_RELATIONSHIP()
);
#214=(
REPRESENTATION_RELATIONSHIP($,$,#14787,#14784)
REPRESENTATION_RELATIONSHIP_WITH_TRANSFORMATION(#102)
SHAPE_REPRESENTATION_RELATIONSHIP()
);
#215=(
REPRESENTATION_RELATIONSHIP($,$,#14788,#14784)
REPRESENTATION_RELATIONSHIP_WITH_TRANSFORMATION(#103)
SHAPE_REPRESENTATION_RELATIONSHIP()
);
#216=(
REPRESENTATION_RELATIONSHIP($,$,#14789,#14784)
REPRESENTATION_RELATIONSHIP_WITH_TRANSFORMATION(#104)
SHAPE_REPRESENTATION_RELATIONSHIP()
);
#217=(
REPRESENTATION_RELATIONSHIP($,$,#14790,#14784)
REPRESENTATION_RELATIONSHIP_WITH_TRANSFORMATION(#105)
SHAPE_REPRESENTATION_RELATIONSHIP()
);
#218=(
REPRESENTATION_RELATIONSHIP($,$,#14791,#14784)
REPRESENTATION_RELATIONSHIP_WITH_TRANSFORMATION(#106)
SHAPE_REPRESENTATION_RELATIONSHIP()
);
#219=(
REPRESENTATION_RELATIONSHIP($,$,#14792,#14784)
REPRESENTATION_RELATIONSHIP_WITH_TRANSFORMATION(#107)
SHAPE_REPRESENTATION_RELATIONSHIP()
);
#220=(
REPRESENTATION_RELATIONSHIP($,$,#14793,#14784)
REPRESENTATION_RELATIONSHIP_WITH_TRANSFORMATION(#108)
SHAPE_REPRESENTATION_RELATIONSHIP()
);
#221=(
REPRESENTATION_RELATIONSHIP($,$,#14794,#14784)
REPRESENTATION_RELATIONSHIP_WITH_TRANSFORMATION(#109)
SHAPE_REPRESENTATION_RELATIONSHIP()
);
#222=(
REPRESENTATION_RELATIONSHIP($,$,#14795,#14784)
REPRESENTATION_RELATIONSHIP_WITH_TRANSFORMATION(#110)
SHAPE_REPRESENTATION_RELATIONSHIP()
);
#223=(
REPRESENTATION_RELATIONSHIP($,$,#14796,#14784)
REPRESENTATION_RELATIONSHIP_WITH_TRANSFORMATION(#111)
SHAPE_REPRESENTATION_RELATIONSHIP()
);
#224=(
REPRESENTATION_RELATIONSHIP($,$,#14796,#14784)
REPRESENTATION_RELATIONSHIP_WITH_TRANSFORMATION(#112)
SHAPE_REPRESENTATION_RELATIONSHIP()
);
#225=(
REPRESENTATION_RELATIONSHIP($,$,#14796,#14784)
REPRESENTATION_RELATIONSHIP_WITH_TRANSFORMATION(#113)
SHAPE_REPRESENTATION_RELATIONSHIP()
);
#226=(
REPRESENTATION_RELATIONSHIP($,$,#14796,#14784)
REPRESENTATION_RELATIONSHIP_WITH_TRANSFORMATION(#114)
SHAPE_REPRESENTATION_RELATIONSHIP()
);
#227=(
REPRESENTATION_RELATIONSHIP($,$,#14796,#14784)
REPRESENTATION_RELATIONSHIP_WITH_TRANSFORMATION(#115)
SHAPE_REPRESENTATION_RELATIONSHIP()
);
#228=(
REPRESENTATION_RELATIONSHIP($,$,#14796,#14784)
REPRESENTATION_RELATIONSHIP_WITH_TRANSFORMATION(#116)
SHAPE_REPRESENTATION_RELATIONSHIP()
);
#229=(
REPRESENTATION_RELATIONSHIP($,$,#14796,#14784)
REPRESENTATION_RELATIONSHIP_WITH_TRANSFORMATION(#117)
SHAPE_REPRESENTATION_RELATIONSHIP()
);
#230=(
REPRESENTATION_RELATIONSHIP($,$,#14796,#14784)
REPRESENTATION_RELATIONSHIP_WITH_TRANSFORMATION(#118)
SHAPE_REPRESENTATION_RELATIONSHIP()
);
#231=(
REPRESENTATION_RELATIONSHIP($,$,#14742,#14741)
REPRESENTATION_RELATIONSHIP_WITH_TRANSFORMATION(#119)
SHAPE_REPRESENTATION_RELATIONSHIP()
);
#232=(
REPRESENTATION_RELATIONSHIP($,$,#14760,#14741)
REPRESENTATION_RELATIONSHIP_WITH_TRANSFORMATION(#120)
SHAPE_REPRESENTATION_RELATIONSHIP()
);
#233=(
REPRESENTATION_RELATIONSHIP($,$,#14769,#14741)
REPRESENTATION_RELATIONSHIP_WITH_TRANSFORMATION(#121)
SHAPE_REPRESENTATION_RELATIONSHIP()
);
#234=(
REPRESENTATION_RELATIONSHIP($,$,#14784,#14741)
REPRESENTATION_RELATIONSHIP_WITH_TRANSFORMATION(#122)
SHAPE_REPRESENTATION_RELATIONSHIP()
);
#235=CONTEXT_DEPENDENT_SHAPE_REPRESENTATION(#123,#14615);
#236=CONTEXT_DEPENDENT_SHAPE_REPRESENTATION(#124,#14616);
#237=CONTEXT_DEPENDENT_SHAPE_REPRESENTATION(#125,#14617);
#238=CONTEXT_DEPENDENT_SHAPE_REPRESENTATION(#126,#14618);
#239=CONTEXT_DEPENDENT_SHAPE_REPRESENTATION(#127,#14619);
#240=CONTEXT_DEPENDENT_SHAPE_REPRESENTATION(#128,#14621);
#241=CONTEXT_DEPENDENT_SHAPE_REPRESENTATION(#129,#14622);
#242=CONTEXT_DEPENDENT_SHAPE_REPRESENTATION(#130,#14623);
#243=CONTEXT_DEPENDENT_SHAPE_REPRESENTATION(#131,#14624);
#244=CONTEXT_DEPENDENT_SHAPE_REPRESENTATION(#132,#14625);
#245=CONTEXT_DEPENDENT_SHAPE_REPRESENTATION(#133,#14626);
#246=CONTEXT_DEPENDENT_SHAPE_REPRESENTATION(#134,#14627);
#247=CONTEXT_DEPENDENT_SHAPE_REPRESENTATION(#135,#14628);
#248=CONTEXT_DEPENDENT_SHAPE_REPRESENTATION(#136,#14629);
#249=CONTEXT_DEPENDENT_SHAPE_REPRESENTATION(#137,#14630);
#250=CONTEXT_DEPENDENT_SHAPE_REPRESENTATION(#138,#14631);
#251=CONTEXT_DEPENDENT_SHAPE_REPRESENTATION(#139,#14632);
#252=CONTEXT_DEPENDENT_SHAPE_REPRESENTATION(#140,#14633);
#253=CONTEXT_DEPENDENT_SHAPE_REPRESENTATION(#141,#14634);
#254=CONTEXT_DEPENDENT_SHAPE_REPRESENTATION(#142,#14635);
#255=CONTEXT_DEPENDENT_SHAPE_REPRESENTATION(#143,#14636);
#256=CONTEXT_DEPENDENT_SHAPE_REPRESENTATION(#144,#14637);
#257=CONTEXT_DEPENDENT_SHAPE_REPRESENTATION(#145,#14638);
#258=CONTEXT_DEPENDENT_SHAPE_REPRESENTATION(#146,#14639);
#259=CONTEXT_DEPENDENT_SHAPE_REPRESENTATION(#147,#14640);
#260=CONTEXT_DEPENDENT_SHAPE_REPRESENTATION(#148,#14641);
#261=CONTEXT_DEPENDENT_SHAPE_REPRESENTATION(#149,#14642);
#262=CONTEXT_DEPENDENT_SHAPE_REPRESENTATION(#150,#14643);
#263=CONTEXT_DEPENDENT_SHAPE_REPRESENTATION(#151,#14644);
#264=CONTEXT_DEPENDENT_SHAPE_REPRESENTATION(#152,#14645);
#265=CONTEXT_DEPENDENT_SHAPE_REPRESENTATION(#153,#14646);
#266=CONTEXT_DEPENDENT_SHAPE_REPRESENTATION(#154,#14647);
#267=CONTEXT_DEPENDENT_SHAPE_REPRESENTATION(#155,#14648);
#268=CONTEXT_DEPENDENT_SHAPE_REPRESENTATION(#156,#14649);
#269=CONTEXT_DEPENDENT_SHAPE_REPRESENTATION(#157,#14650);
#270=CONTEXT_DEPENDENT_SHAPE_REPRESENTATION(#158,#14651);
#271=CONTEXT_DEPENDENT_SHAPE_REPRESENTATION(#159,#14652);
#272=CONTEXT_DEPENDENT_SHAPE_REPRESENTATION(#160,#14653);
#273=CONTEXT_DEPENDENT_SHAPE_REPRESENTATION(#161,#14654);
#274=CONTEXT_DEPENDENT_SHAPE_REPRESENTATION(#162,#14655);
#275=CONTEXT_DEPENDENT_SHAPE_REPRESENTATION(#163,#14656);
#276=CONTEXT_DEPENDENT_SHAPE_REPRESENTATION(#164,#14657);
#277=CONTEXT_DEPENDENT_SHAPE_REPRESENTATION(#165,#14658);
#278=CONTEXT_DEPENDENT_SHAPE_REPRESENTATION(#166,#14659);
#279=CONTEXT_DEPENDENT_SHAPE_REPRESENTATION(#167,#14660);
#280=CONTEXT_DEPENDENT_SHAPE_REPRESENTATION(#168,#14661);
#281=CONTEXT_DEPENDENT_SHAPE_REPRESENTATION(#169,#14662);
#282=CONTEXT_DEPENDENT_SHAPE_REPRESENTATION(#170,#14663);
#283=CONTEXT_DEPENDENT_SHAPE_REPRESENTATION(#171,#14664);
#284=CONTEXT_DEPENDENT_SHAPE_REPRESENTATION(#172,#14665);
#285=CONTEXT_DEPENDENT_SHAPE_REPRESENTATION(#173,#14666);
#286=CONTEXT_DEPENDENT_SHAPE_REPRESENTATION(#174,#14667);
#287=CONTEXT_DEPENDENT_SHAPE_REPRESENTATION(#175,#14668);
#288=CONTEXT_DEPENDENT_SHAPE_REPRESENTATION(#176,#14669);
#289=CONTEXT_DEPENDENT_SHAPE_REPRESENTATION(#177,#14670);
#290=CONTEXT_DEPENDENT_SHAPE_REPRESENTATION(#178,#14671);
#291=CONTEXT_DEPENDENT_SHAPE_REPRESENTATION(#179,#14672);
#292=CONTEXT_DEPENDENT_SHAPE_REPRESENTATION(#180,#14673);
#293=CONTEXT_DEPENDENT_SHAPE_REPRESENTATION(#181,#14674);
#294=CONTEXT_DEPENDENT_SHAPE_REPRESENTATION(#182,#14675);
#295=CONTEXT_DEPENDENT_SHAPE_REPRESENTATION(#183,#14689);
#296=CONTEXT_DEPENDENT_SHAPE_REPRESENTATION(#184,#14690);
#297=CONTEXT_DEPENDENT_SHAPE_REPRESENTATION(#185,#14691);
#298=CONTEXT_DEPENDENT_SHAPE_REPRESENTATION(#186,#14692);
#299=CONTEXT_DEPENDENT_SHAPE_REPRESENTATION(#187,#14693);
#300=CONTEXT_DEPENDENT_SHAPE_REPRESENTATION(#188,#14694);
#301=CONTEXT_DEPENDENT_SHAPE_REPRESENTATION(#189,#14695);
#302=CONTEXT_DEPENDENT_SHAPE_REPRESENTATION(#190,#14696);
#303=CONTEXT_DEPENDENT_SHAPE_REPRESENTATION(#191,#14697);
#304=CONTEXT_DEPENDENT_SHAPE_REPRESENTATION(#192,#14698);
#305=CONTEXT_DEPENDENT_SHAPE_REPRESENTATION(#193,#14699);
#306=CONTEXT_DEPENDENT_SHAPE_REPRESENTATION(#194,#14700);
#307=CONTEXT_DEPENDENT_SHAPE_REPRESENTATION(#195,#14701);
#308=CONTEXT_DEPENDENT_SHAPE_REPRESENTATION(#196,#14702);
#309=CONTEXT_DEPENDENT_SHAPE_REPRESENTATION(#197,#14703);
#310=CONTEXT_DEPENDENT_SHAPE_REPRESENTATION(#198,#14704);
#311=CONTEXT_DEPENDENT_SHAPE_REPRESENTATION(#199,#14705);
#312=CONTEXT_DEPENDENT_SHAPE_REPRESENTATION(#200,#14706);
#313=CONTEXT_DEPENDENT_SHAPE_REPRESENTATION(#201,#14707);
#314=CONTEXT_DEPENDENT_SHAPE_REPRESENTATION(#202,#14708);
#315=CONTEXT_DEPENDENT_SHAPE_REPRESENTATION(#203,#14709);
#316=CONTEXT_DEPENDENT_SHAPE_REPRESENTATION(#204,#14710);
#317=CONTEXT_DEPENDENT_SHAPE_REPRESENTATION(#205,#14711);
#318=CONTEXT_DEPENDENT_SHAPE_REPRESENTATION(#206,#14712);
#319=CONTEXT_DEPENDENT_SHAPE_REPRESENTATION(#207,#14713);
#320=CONTEXT_DEPENDENT_SHAPE_REPRESENTATION(#208,#14714);
#321=CONTEXT_DEPENDENT_SHAPE_REPRESENTATION(#209,#14715);
#322=CONTEXT_DEPENDENT_SHAPE_REPRESENTATION(#210,#14716);
#323=CONTEXT_DEPENDENT_SHAPE_REPRESENTATION(#211,#14717);
#324=CONTEXT_DEPENDENT_SHAPE_REPRESENTATION(#212,#14718);
#325=CONTEXT_DEPENDENT_SHAPE_REPRESENTATION(#213,#14719);
#326=CONTEXT_DEPENDENT_SHAPE_REPRESENTATION(#214,#14720);
#327=CONTEXT_DEPENDENT_SHAPE_REPRESENTATION(#215,#14721);
#328=CONTEXT_DEPENDENT_SHAPE_REPRESENTATION(#216,#14722);
#329=CONTEXT_DEPENDENT_SHAPE_REPRESENTATION(#217,#14723);
#330=CONTEXT_DEPENDENT_SHAPE_REPRESENTATION(#218,#14724);
#331=CONTEXT_DEPENDENT_SHAPE_REPRESENTATION(#219,#14725);
#332=CONTEXT_DEPENDENT_SHAPE_REPRESENTATION(#220,#14726);
#333=CONTEXT_DEPENDENT_SHAPE_REPRESENTATION(#221,#14727);
#334=CONTEXT_DEPENDENT_SHAPE_REPRESENTATION(#222,#14728);
#335=CONTEXT_DEPENDENT_SHAPE_REPRESENTATION(#223,#14729);
#336=CONTEXT_DEPENDENT_SHAPE_REPRESENTATION(#224,#14730);
#337=CONTEXT_DEPENDENT_SHAPE_REPRESENTATION(#225,#14731);
#338=CONTEXT_DEPENDENT_SHAPE_REPRESENTATION(#226,#14732);
#339=CONTEXT_DEPENDENT_SHAPE_REPRESENTATION(#227,#14733);
#340=CONTEXT_DEPENDENT_SHAPE_REPRESENTATION(#228,#14734);
#341=CONTEXT_DEPENDENT_SHAPE_REPRESENTATION(#229,#14735);
#342=CONTEXT_DEPENDENT_SHAPE_REPRESENTATION(#230,#14736);
#343=CONTEXT_DEPENDENT_SHAPE_REPRESENTATION(#231,#14737);
#344=CONTEXT_DEPENDENT_SHAPE_REPRESENTATION(#232,#14738);
#345=CONTEXT_DEPENDENT_SHAPE_REPRESENTATION(#233,#14739);
#346=CONTEXT_DEPENDENT_SHAPE_REPRESENTATION(#234,#14740);
#347=NEXT_ASSEMBLY_USAGE_OCCURRENCE('Inner ring:1','Inner ring:1',
'Inner ring:1',#14834,#14835,'Inner ring:1');
#348=NEXT_ASSEMBLY_USAGE_OCCURRENCE('Outer ring:1','Outer ring:1',
'Outer ring:1',#14834,#14836,'Outer ring:1');
#349=NEXT_ASSEMBLY_USAGE_OCCURRENCE('Balls:1','Balls:1','Balls:1',#14834,
#14837,'Balls:1');
#350=NEXT_ASSEMBLY_USAGE_OCCURRENCE('Cage:1','Cage:1','Cage:1',#14834,#14838,
'Cage:1');
#351=NEXT_ASSEMBLY_USAGE_OCCURRENCE('Seals 2RS:1','Seals 2RS:1',
'Seals 2RS:1',#14834,#14839,'Seals 2RS:1');
#352=NEXT_ASSEMBLY_USAGE_OCCURRENCE('200 mm arm:1','200 mm arm:1',
'200 mm arm:1',#14817,#14818,'200 mm arm:1');
#353=NEXT_ASSEMBLY_USAGE_OCCURRENCE('Outer race spacer:1',
'Outer race spacer:1','Outer race spacer:1',#14817,#14819,
'Outer race spacer:1');
#354=NEXT_ASSEMBLY_USAGE_OCCURRENCE('Bearing cap:1','Bearing cap:1',
'Bearing cap:1',#14817,#14820,'Bearing cap:1');
#355=NEXT_ASSEMBLY_USAGE_OCCURRENCE('Bearing cap (1):1',
'Bearing cap (1):1','Bearing cap (1):1',#14817,#14821,
'Bearing cap (1):1');
#356=NEXT_ASSEMBLY_USAGE_OCCURRENCE('Outer race spacer (1):1',
'Outer race spacer (1):1','Outer race spacer (1):1',#14817,#14822,
'Outer race spacer (1):1');
#357=NEXT_ASSEMBLY_USAGE_OCCURRENCE('Bearing cap (2):1',
'Bearing cap (2):1','Bearing cap (2):1',#14817,#14823,
'Bearing cap (2):1');
#358=NEXT_ASSEMBLY_USAGE_OCCURRENCE('Bearing cap (3):1',
'Bearing cap (3):1','Bearing cap (3):1',#14817,#14824,
'Bearing cap (3):1');
#359=NEXT_ASSEMBLY_USAGE_OCCURRENCE('Moving spring anchor:1',
'Moving spring anchor:1','Moving spring anchor:1',#14817,#14825,
'Moving spring anchor:1');
#360=NEXT_ASSEMBLY_USAGE_OCCURRENCE(
'Sealed Ball Bearing - 10 x 30 x 9 mm:2',
'Sealed Ball Bearing - 10 x 30 x 9 mm:2',
'Sealed Ball Bearing - 10 x 30 x 9 mm:2',#14817,#14834,
'Sealed Ball Bearing - 10 x 30 x 9 mm:2');
#361=NEXT_ASSEMBLY_USAGE_OCCURRENCE(
'Sealed Ball Bearing - 10 x 30 x 9 mm:3',
'Sealed Ball Bearing - 10 x 30 x 9 mm:3',
'Sealed Ball Bearing - 10 x 30 x 9 mm:3',#14817,#14834,
'Sealed Ball Bearing - 10 x 30 x 9 mm:3');
#362=NEXT_ASSEMBLY_USAGE_OCCURRENCE('M4x10 Cap Screw:2',
'M4x10 Cap Screw:2','M4x10 Cap Screw:2',#14817,#14840,
'M4x10 Cap Screw:2');
#363=NEXT_ASSEMBLY_USAGE_OCCURRENCE('M4x10 Cap Screw:3',
'M4x10 Cap Screw:3','M4x10 Cap Screw:3',#14817,#14840,
'M4x10 Cap Screw:3');
#364=NEXT_ASSEMBLY_USAGE_OCCURRENCE('M4x10 Cap Screw:4',
'M4x10 Cap Screw:4','M4x10 Cap Screw:4',#14817,#14840,
'M4x10 Cap Screw:4');
#365=NEXT_ASSEMBLY_USAGE_OCCURRENCE('M4x10 Cap Screw:5',
'M4x10 Cap Screw:5','M4x10 Cap Screw:5',#14817,#14840,
'M4x10 Cap Screw:5');
#366=NEXT_ASSEMBLY_USAGE_OCCURRENCE('M4x10 Cap Screw:6',
'M4x10 Cap Screw:6','M4x10 Cap Screw:6',#14817,#14840,
'M4x10 Cap Screw:6');
#367=NEXT_ASSEMBLY_USAGE_OCCURRENCE('M4x10 Cap Screw:7',
'M4x10 Cap Screw:7','M4x10 Cap Screw:7',#14817,#14840,
'M4x10 Cap Screw:7');
#368=NEXT_ASSEMBLY_USAGE_OCCURRENCE('M4x10 Cap Screw:8',
'M4x10 Cap Screw:8','M4x10 Cap Screw:8',#14817,#14840,
'M4x10 Cap Screw:8');
#369=NEXT_ASSEMBLY_USAGE_OCCURRENCE('M4x10 Cap Screw:9',
'M4x10 Cap Screw:9','M4x10 Cap Screw:9',#14817,#14840,
'M4x10 Cap Screw:9');
#370=NEXT_ASSEMBLY_USAGE_OCCURRENCE(
'Sealed Ball Bearing - 10 x 30 x 9 mm:4',
'Sealed Ball Bearing - 10 x 30 x 9 mm:4',
'Sealed Ball Bearing - 10 x 30 x 9 mm:4',#14817,#14834,
'Sealed Ball Bearing - 10 x 30 x 9 mm:4');
#371=NEXT_ASSEMBLY_USAGE_OCCURRENCE(
'Sealed Ball Bearing - 10 x 30 x 9 mm:5',
'Sealed Ball Bearing - 10 x 30 x 9 mm:5',
'Sealed Ball Bearing - 10 x 30 x 9 mm:5',#14817,#14834,
'Sealed Ball Bearing - 10 x 30 x 9 mm:5');
#372=NEXT_ASSEMBLY_USAGE_OCCURRENCE('M4x10 Cap Screw:10',
'M4x10 Cap Screw:10','M4x10 Cap Screw:10',#14817,#14840,
'M4x10 Cap Screw:10');
#373=NEXT_ASSEMBLY_USAGE_OCCURRENCE('M4x10 Cap Screw:11',
'M4x10 Cap Screw:11','M4x10 Cap Screw:11',#14817,#14840,
'M4x10 Cap Screw:11');
#374=NEXT_ASSEMBLY_USAGE_OCCURRENCE('M4x10 Cap Screw:12',
'M4x10 Cap Screw:12','M4x10 Cap Screw:12',#14817,#14840,
'M4x10 Cap Screw:12');
#375=NEXT_ASSEMBLY_USAGE_OCCURRENCE('M4x10 Cap Screw:13',
'M4x10 Cap Screw:13','M4x10 Cap Screw:13',#14817,#14840,
'M4x10 Cap Screw:13');
#376=NEXT_ASSEMBLY_USAGE_OCCURRENCE('M4x10 Cap Screw:14',
'M4x10 Cap Screw:14','M4x10 Cap Screw:14',#14817,#14840,
'M4x10 Cap Screw:14');
#377=NEXT_ASSEMBLY_USAGE_OCCURRENCE('M4x10 Cap Screw:15',
'M4x10 Cap Screw:15','M4x10 Cap Screw:15',#14817,#14840,
'M4x10 Cap Screw:15');
#378=NEXT_ASSEMBLY_USAGE_OCCURRENCE('M4x10 Cap Screw:16',
'M4x10 Cap Screw:16','M4x10 Cap Screw:16',#14817,#14840,
'M4x10 Cap Screw:16');
#379=NEXT_ASSEMBLY_USAGE_OCCURRENCE('M4x10 Cap Screw:17',
'M4x10 Cap Screw:17','M4x10 Cap Screw:17',#14817,#14840,
'M4x10 Cap Screw:17');
#380=NEXT_ASSEMBLY_USAGE_OCCURRENCE('200 mm arm (1):1',
'200 mm arm (1):1','200 mm arm (1):1',#14826,#14827,'200 mm arm (1):1');
#381=NEXT_ASSEMBLY_USAGE_OCCURRENCE('Outer race spacer (2):1',
'Outer race spacer (2):1','Outer race spacer (2):1',#14826,#14828,
'Outer race spacer (2):1');
#382=NEXT_ASSEMBLY_USAGE_OCCURRENCE('Bearing cap (4):1',
'Bearing cap (4):1','Bearing cap (4):1',#14826,#14829,
'Bearing cap (4):1');
#383=NEXT_ASSEMBLY_USAGE_OCCURRENCE('Bearing cap (5):1',
'Bearing cap (5):1','Bearing cap (5):1',#14826,#14830,
'Bearing cap (5):1');
#384=NEXT_ASSEMBLY_USAGE_OCCURRENCE('Outer race spacer (3):1',
'Outer race spacer (3):1','Outer race spacer (3):1',#14826,#14831,
'Outer race spacer (3):1');
#385=NEXT_ASSEMBLY_USAGE_OCCURRENCE('Bearing cap (6):1',
'Bearing cap (6):1','Bearing cap (6):1',#14826,#14832,
'Bearing cap (6):1');
#386=NEXT_ASSEMBLY_USAGE_OCCURRENCE('Bearing cap (7):1',
'Bearing cap (7):1','Bearing cap (7):1',#14826,#14833,
'Bearing cap (7):1');
#387=NEXT_ASSEMBLY_USAGE_OCCURRENCE(
'Sealed Ball Bearing - 10 x 30 x 9 mm:6',
'Sealed Ball Bearing - 10 x 30 x 9 mm:6',
'Sealed Ball Bearing - 10 x 30 x 9 mm:6',#14826,#14834,
'Sealed Ball Bearing - 10 x 30 x 9 mm:6');
#388=NEXT_ASSEMBLY_USAGE_OCCURRENCE(
'Sealed Ball Bearing - 10 x 30 x 9 mm:7',
'Sealed Ball Bearing - 10 x 30 x 9 mm:7',
'Sealed Ball Bearing - 10 x 30 x 9 mm:7',#14826,#14834,
'Sealed Ball Bearing - 10 x 30 x 9 mm:7');
#389=NEXT_ASSEMBLY_USAGE_OCCURRENCE('M4x10 Cap Screw:18',
'M4x10 Cap Screw:18','M4x10 Cap Screw:18',#14826,#14840,
'M4x10 Cap Screw:18');
#390=NEXT_ASSEMBLY_USAGE_OCCURRENCE('M4x10 Cap Screw:19',
'M4x10 Cap Screw:19','M4x10 Cap Screw:19',#14826,#14840,
'M4x10 Cap Screw:19');
#391=NEXT_ASSEMBLY_USAGE_OCCURRENCE('M4x10 Cap Screw:20',
'M4x10 Cap Screw:20','M4x10 Cap Screw:20',#14826,#14840,
'M4x10 Cap Screw:20');
#392=NEXT_ASSEMBLY_USAGE_OCCURRENCE('M4x10 Cap Screw:21',
'M4x10 Cap Screw:21','M4x10 Cap Screw:21',#14826,#14840,
'M4x10 Cap Screw:21');
#393=NEXT_ASSEMBLY_USAGE_OCCURRENCE('M4x10 Cap Screw:22',
'M4x10 Cap Screw:22','M4x10 Cap Screw:22',#14826,#14840,
'M4x10 Cap Screw:22');
#394=NEXT_ASSEMBLY_USAGE_OCCURRENCE('M4x10 Cap Screw:23',
'M4x10 Cap Screw:23','M4x10 Cap Screw:23',#14826,#14840,
'M4x10 Cap Screw:23');
#395=NEXT_ASSEMBLY_USAGE_OCCURRENCE('M4x10 Cap Screw:24',
'M4x10 Cap Screw:24','M4x10 Cap Screw:24',#14826,#14840,
'M4x10 Cap Screw:24');
#396=NEXT_ASSEMBLY_USAGE_OCCURRENCE('M4x10 Cap Screw:25',
'M4x10 Cap Screw:25','M4x10 Cap Screw:25',#14826,#14840,
'M4x10 Cap Screw:25');
#397=NEXT_ASSEMBLY_USAGE_OCCURRENCE(
'Sealed Ball Bearing - 10 x 30 x 9 mm:8',
'Sealed Ball Bearing - 10 x 30 x 9 mm:8',
'Sealed Ball Bearing - 10 x 30 x 9 mm:8',#14826,#14834,
'Sealed Ball Bearing - 10 x 30 x 9 mm:8');
#398=NEXT_ASSEMBLY_USAGE_OCCURRENCE(
'Sealed Ball Bearing - 10 x 30 x 9 mm:9',
'Sealed Ball Bearing - 10 x 30 x 9 mm:9',
'Sealed Ball Bearing - 10 x 30 x 9 mm:9',#14826,#14834,
'Sealed Ball Bearing - 10 x 30 x 9 mm:9');
#399=NEXT_ASSEMBLY_USAGE_OCCURRENCE('M4x10 Cap Screw:26',
'M4x10 Cap Screw:26','M4x10 Cap Screw:26',#14826,#14840,
'M4x10 Cap Screw:26');
#400=NEXT_ASSEMBLY_USAGE_OCCURRENCE('M4x10 Cap Screw:27',
'M4x10 Cap Screw:27','M4x10 Cap Screw:27',#14826,#14840,
'M4x10 Cap Screw:27');
#401=NEXT_ASSEMBLY_USAGE_OCCURRENCE('M4x10 Cap Screw:28',
'M4x10 Cap Screw:28','M4x10 Cap Screw:28',#14826,#14840,
'M4x10 Cap Screw:28');
#402=NEXT_ASSEMBLY_USAGE_OCCURRENCE('M4x10 Cap Screw:29',
'M4x10 Cap Screw:29','M4x10 Cap Screw:29',#14826,#14840,
'M4x10 Cap Screw:29');
#403=NEXT_ASSEMBLY_USAGE_OCCURRENCE('M4x10 Cap Screw:30',
'M4x10 Cap Screw:30','M4x10 Cap Screw:30',#14826,#14840,
'M4x10 Cap Screw:30');
#404=NEXT_ASSEMBLY_USAGE_OCCURRENCE('M4x10 Cap Screw:31',
'M4x10 Cap Screw:31','M4x10 Cap Screw:31',#14826,#14840,
'M4x10 Cap Screw:31');
#405=NEXT_ASSEMBLY_USAGE_OCCURRENCE('M4x10 Cap Screw:32',
'M4x10 Cap Screw:32','M4x10 Cap Screw:32',#14826,#14840,
'M4x10 Cap Screw:32');
#406=NEXT_ASSEMBLY_USAGE_OCCURRENCE('M4x10 Cap Screw:33',
'M4x10 Cap Screw:33','M4x10 Cap Screw:33',#14826,#14840,
'M4x10 Cap Screw:33');
#407=NEXT_ASSEMBLY_USAGE_OCCURRENCE('Base:1','Base:1','Base:1',#14799,#14800,
'Base:1');
#408=NEXT_ASSEMBLY_USAGE_OCCURRENCE('Foot strip:1','Foot strip:1',
'Foot strip:1',#14799,#14801,'Foot strip:1');
#409=NEXT_ASSEMBLY_USAGE_OCCURRENCE('Foot strip (1):1',
'Foot strip (1):1','Foot strip (1):1',#14799,#14802,'Foot strip (1):1');
#410=NEXT_ASSEMBLY_USAGE_OCCURRENCE('Fixed link:1','Fixed link:1',
'Fixed link:1',#14799,#14803,'Fixed link:1');
#411=NEXT_ASSEMBLY_USAGE_OCCURRENCE('Spring arbor pivot:1',
'Spring arbor pivot:1','Spring arbor pivot:1',#14799,#14804,
'Spring arbor pivot:1');
#412=NEXT_ASSEMBLY_USAGE_OCCURRENCE('Inner race sleeve:1',
'Inner race sleeve:1','Inner race sleeve:1',#14799,#14805,
'Inner race sleeve:1');
#413=NEXT_ASSEMBLY_USAGE_OCCURRENCE('Rear inner spacer:1',
'Rear inner spacer:1','Rear inner spacer:1',#14799,#14806,
'Rear inner spacer:1');
#414=NEXT_ASSEMBLY_USAGE_OCCURRENCE('Long front spacer:1',
'Long front spacer:1','Long front spacer:1',#14799,#14807,
'Long front spacer:1');
#415=NEXT_ASSEMBLY_USAGE_OCCURRENCE('Pivot keeper:1','Pivot keeper:1',
'Pivot keeper:1',#14799,#14808,'Pivot keeper:1');
#416=NEXT_ASSEMBLY_USAGE_OCCURRENCE('Pivot pin:1','Pivot pin:1',
'Pivot pin:1',#14799,#14809,'Pivot pin:1');
#417=NEXT_ASSEMBLY_USAGE_OCCURRENCE('Inner race sleeve (1):1',
'Inner race sleeve (1):1','Inner race sleeve (1):1',#14799,#14810,
'Inner race sleeve (1):1');
#418=NEXT_ASSEMBLY_USAGE_OCCURRENCE('Rear inner spacer (1):1',
'Rear inner spacer (1):1','Rear inner spacer (1):1',#14799,#14811,
'Rear inner spacer (1):1');
#419=NEXT_ASSEMBLY_USAGE_OCCURRENCE('Front spacer:1','Front spacer:1',
'Front spacer:1',#14799,#14812,'Front spacer:1');
#420=NEXT_ASSEMBLY_USAGE_OCCURRENCE('Pivot keeper (1):1',
'Pivot keeper (1):1','Pivot keeper (1):1',#14799,#14813,
'Pivot keeper (1):1');
#421=NEXT_ASSEMBLY_USAGE_OCCURRENCE('Fixed spring bracket:1',
'Fixed spring bracket:1','Fixed spring bracket:1',#14799,#14814,
'Fixed spring bracket:1');
#422=NEXT_ASSEMBLY_USAGE_OCCURRENCE('Installed torsion spring:1',
'Installed torsion spring:1','Installed torsion spring:1',#14799,#14815,
'Installed torsion spring:1');
#423=NEXT_ASSEMBLY_USAGE_OCCURRENCE('M5x14 Cap Screw:2',
'M5x14 Cap Screw:2','M5x14 Cap Screw:2',#14799,#14816,
'M5x14 Cap Screw:2');
#424=NEXT_ASSEMBLY_USAGE_OCCURRENCE('M5x14 Cap Screw:3',
'M5x14 Cap Screw:3','M5x14 Cap Screw:3',#14799,#14816,
'M5x14 Cap Screw:3');
#425=NEXT_ASSEMBLY_USAGE_OCCURRENCE('M5x14 Cap Screw:4',
'M5x14 Cap Screw:4','M5x14 Cap Screw:4',#14799,#14816,
'M5x14 Cap Screw:4');
#426=NEXT_ASSEMBLY_USAGE_OCCURRENCE('M5x14 Cap Screw:5',
'M5x14 Cap Screw:5','M5x14 Cap Screw:5',#14799,#14816,
'M5x14 Cap Screw:5');
#427=NEXT_ASSEMBLY_USAGE_OCCURRENCE('Cap Screw - M4x16:2',
'Cap Screw - M4x16:2','Cap Screw - M4x16:2',#14799,#14853,
'Cap Screw - M4x16:2');
#428=NEXT_ASSEMBLY_USAGE_OCCURRENCE('Cap Screw - M4x16:3',
'Cap Screw - M4x16:3','Cap Screw - M4x16:3',#14799,#14853,
'Cap Screw - M4x16:3');
#429=NEXT_ASSEMBLY_USAGE_OCCURRENCE('Cap Screw - M4x16:4',
'Cap Screw - M4x16:4','Cap Screw - M4x16:4',#14799,#14853,
'Cap Screw - M4x16:4');
#430=NEXT_ASSEMBLY_USAGE_OCCURRENCE('Cap Screw - M4x16:5',
'Cap Screw - M4x16:5','Cap Screw - M4x16:5',#14799,#14853,
'Cap Screw - M4x16:5');
#431=NEXT_ASSEMBLY_USAGE_OCCURRENCE('Cap Screw - M4x16:10',
'Cap Screw - M4x16:10','Cap Screw - M4x16:10',#14799,#14853,
'Cap Screw - M4x16:10');
#432=NEXT_ASSEMBLY_USAGE_OCCURRENCE('Cap Screw - M4x16:11',
'Cap Screw - M4x16:11','Cap Screw - M4x16:11',#14799,#14853,
'Cap Screw - M4x16:11');
#433=NEXT_ASSEMBLY_USAGE_OCCURRENCE('Cap Screw - M4x16:12',
'Cap Screw - M4x16:12','Cap Screw - M4x16:12',#14799,#14853,
'Cap Screw - M4x16:12');
#434=NEXT_ASSEMBLY_USAGE_OCCURRENCE('Cap Screw - M4x16:13',
'Cap Screw - M4x16:13','Cap Screw - M4x16:13',#14799,#14853,
'Cap Screw - M4x16:13');
#435=NEXT_ASSEMBLY_USAGE_OCCURRENCE('Cap Screw - M4x16:18',
'Cap Screw - M4x16:18','Cap Screw - M4x16:18',#14799,#14853,
'Cap Screw - M4x16:18');
#436=NEXT_ASSEMBLY_USAGE_OCCURRENCE('Platform link:1','Platform link:1',
'Platform link:1',#14841,#14842,'Platform link:1');
#437=NEXT_ASSEMBLY_USAGE_OCCURRENCE('Pivot pin (1):1','Pivot pin (1):1',
'Pivot pin (1):1',#14841,#14843,'Pivot pin (1):1');
#438=NEXT_ASSEMBLY_USAGE_OCCURRENCE('Inner race sleeve (2):1',
'Inner race sleeve (2):1','Inner race sleeve (2):1',#14841,#14844,
'Inner race sleeve (2):1');
#439=NEXT_ASSEMBLY_USAGE_OCCURRENCE('Rear inner spacer (2):1',
'Rear inner spacer (2):1','Rear inner spacer (2):1',#14841,#14845,
'Rear inner spacer (2):1');
#440=NEXT_ASSEMBLY_USAGE_OCCURRENCE('Front spacer (1):1',
'Front spacer (1):1','Front spacer (1):1',#14841,#14846,
'Front spacer (1):1');
#441=NEXT_ASSEMBLY_USAGE_OCCURRENCE('Pivot keeper (2):1',
'Pivot keeper (2):1','Pivot keeper (2):1',#14841,#14847,
'Pivot keeper (2):1');
#442=NEXT_ASSEMBLY_USAGE_OCCURRENCE('Pivot pin (2):1','Pivot pin (2):1',
'Pivot pin (2):1',#14841,#14848,'Pivot pin (2):1');
#443=NEXT_ASSEMBLY_USAGE_OCCURRENCE('Inner race sleeve (3):1',
'Inner race sleeve (3):1','Inner race sleeve (3):1',#14841,#14849,
'Inner race sleeve (3):1');
#444=NEXT_ASSEMBLY_USAGE_OCCURRENCE('Rear inner spacer (3):1',
'Rear inner spacer (3):1','Rear inner spacer (3):1',#14841,#14850,
'Rear inner spacer (3):1');
#445=NEXT_ASSEMBLY_USAGE_OCCURRENCE('Front spacer (2):1',
'Front spacer (2):1','Front spacer (2):1',#14841,#14851,
'Front spacer (2):1');
#446=NEXT_ASSEMBLY_USAGE_OCCURRENCE('Pivot keeper (3):1',
'Pivot keeper (3):1','Pivot keeper (3):1',#14841,#14852,
'Pivot keeper (3):1');
#447=NEXT_ASSEMBLY_USAGE_OCCURRENCE('Cap Screw - M4x16:6',
'Cap Screw - M4x16:6','Cap Screw - M4x16:6',#14841,#14853,
'Cap Screw - M4x16:6');
#448=NEXT_ASSEMBLY_USAGE_OCCURRENCE('Cap Screw - M4x16:7',
'Cap Screw - M4x16:7','Cap Screw - M4x16:7',#14841,#14853,
'Cap Screw - M4x16:7');
#449=NEXT_ASSEMBLY_USAGE_OCCURRENCE('Cap Screw - M4x16:8',
'Cap Screw - M4x16:8','Cap Screw - M4x16:8',#14841,#14853,
'Cap Screw - M4x16:8');
#450=NEXT_ASSEMBLY_USAGE_OCCURRENCE('Cap Screw - M4x16:9',
'Cap Screw - M4x16:9','Cap Screw - M4x16:9',#14841,#14853,
'Cap Screw - M4x16:9');
#451=NEXT_ASSEMBLY_USAGE_OCCURRENCE('Cap Screw - M4x16:14',
'Cap Screw - M4x16:14','Cap Screw - M4x16:14',#14841,#14853,
'Cap Screw - M4x16:14');
#452=NEXT_ASSEMBLY_USAGE_OCCURRENCE('Cap Screw - M4x16:15',
'Cap Screw - M4x16:15','Cap Screw - M4x16:15',#14841,#14853,
'Cap Screw - M4x16:15');
#453=NEXT_ASSEMBLY_USAGE_OCCURRENCE('Cap Screw - M4x16:16',
'Cap Screw - M4x16:16','Cap Screw - M4x16:16',#14841,#14853,
'Cap Screw - M4x16:16');
#454=NEXT_ASSEMBLY_USAGE_OCCURRENCE('Cap Screw - M4x16:17',
'Cap Screw - M4x16:17','Cap Screw - M4x16:17',#14841,#14853,
'Cap Screw - M4x16:17');
#455=NEXT_ASSEMBLY_USAGE_OCCURRENCE(
'Fixed bracket and counter spring:1',
'Fixed bracket and counter spring:1',
'Fixed bracket and counter spring:1',#14798,#14799,
'Fixed bracket and counter spring:1');
#456=NEXT_ASSEMBLY_USAGE_OCCURRENCE('Lower link:1','Lower link:1',
'Lower link:1',#14798,#14817,'Lower link:1');
#457=NEXT_ASSEMBLY_USAGE_OCCURRENCE('Upper link:1','Upper link:1',
'Upper link:1',#14798,#14826,'Upper link:1');
#458=NEXT_ASSEMBLY_USAGE_OCCURRENCE('Level platform link:1',
'Level platform link:1','Level platform link:1',#14798,#14841,
'Level platform link:1');
#459=SPHERICAL_SURFACE('',#8548,0.23815);
#460=SPHERICAL_SURFACE('',#8550,0.23815);
#461=SPHERICAL_SURFACE('',#8552,0.23815);
#462=SPHERICAL_SURFACE('',#8554,0.23815);
#463=SPHERICAL_SURFACE('',#8556,0.23815);
#464=SPHERICAL_SURFACE('',#8558,0.23815);
#465=SPHERICAL_SURFACE('',#8560,0.23815);
#466=SPHERICAL_SURFACE('',#8562,0.23815);
#467=SPHERICAL_SURFACE('',#8565,0.247676);
#468=SPHERICAL_SURFACE('',#8581,0.247676);
#469=SPHERICAL_SURFACE('',#8586,0.247676);
#470=SPHERICAL_SURFACE('',#8591,0.247676);
#471=SPHERICAL_SURFACE('',#8596,0.247676);
#472=SPHERICAL_SURFACE('',#8601,0.247676);
#473=SPHERICAL_SURFACE('',#8606,0.247676);
#474=SPHERICAL_SURFACE('',#8614,0.247676);
#475=TOROIDAL_SURFACE('',#8508,1.,0.247676);
#476=TOROIDAL_SURFACE('',#8528,1.,0.247676);
#477=CONICAL_SURFACE('',#8197,0.4,0.785398163397448);
#478=CONICAL_SURFACE('',#8201,0.41,0.785398163397448);
#479=CONICAL_SURFACE('',#8205,0.26,0.463647609000806);
#480=CONICAL_SURFACE('',#8519,0.53,0.785398163397448);
#481=CONICAL_SURFACE('',#8526,0.53,0.785398163397448);
#482=CONICAL_SURFACE('',#8539,1.47,0.785398163397449);
#483=CONICAL_SURFACE('',#8543,1.47,0.785398163397449);
#484=CONICAL_SURFACE('',#8653,0.325,0.785398163397448);
#485=CONICAL_SURFACE('',#8657,0.335,0.785398163397448);
#486=CONICAL_SURFACE('',#8661,0.21,0.463647609000806);
#487=CONICAL_SURFACE('',#8895,0.325,0.785398163397448);
#488=CONICAL_SURFACE('',#8899,0.335,0.785398163397448);
#489=CONICAL_SURFACE('',#8903,0.21,0.463647609000806);
#490=CONICAL_SURFACE('',#8907,0.18,0.785398163397448);
#491=ORIENTED_CLOSED_SHELL('',*,#7342,.F.);
#492=ORIENTED_CLOSED_SHELL('',*,#7372,.F.);
#493=ORIENTED_CLOSED_SHELL('',*,#7386,.F.);
#494=BREP_WITH_VOIDS('Body1',#7343,(#491));
#495=BREP_WITH_VOIDS('Body1',#7373,(#492));
#496=BREP_WITH_VOIDS('Body1',#7385,(#493));
#497=B_SPLINE_SURFACE_WITH_KNOTS('',3,3,((#12064,#12065,#12066,#12067,#12068,
#12069,#12070,#12071,#12072,#12073,#12074,#12075,#12076,#12077,#12078,#12079,
#12080,#12081,#12082,#12083,#12084,#12085,#12086,#12087,#12088,#12089,#12090,
#12091,#12092,#12093,#12094,#12095,#12096,#12097,#12098,#12099,#12100,#12101,
#12102,#12103,#12104),(#12105,#12106,#12107,#12108,#12109,#12110,#12111,
#12112,#12113,#12114,#12115,#12116,#12117,#12118,#12119,#12120,#12121,#12122,
#12123,#12124,#12125,#12126,#12127,#12128,#12129,#12130,#12131,#12132,#12133,
#12134,#12135,#12136,#12137,#12138,#12139,#12140,#12141,#12142,#12143,#12144,
#12145),(#12146,#12147,#12148,#12149,#12150,#12151,#12152,#12153,#12154,
#12155,#12156,#12157,#12158,#12159,#12160,#12161,#12162,#12163,#12164,#12165,
#12166,#12167,#12168,#12169,#12170,#12171,#12172,#12173,#12174,#12175,#12176,
#12177,#12178,#12179,#12180,#12181,#12182,#12183,#12184,#12185,#12186),
(#12187,#12188,#12189,#12190,#12191,#12192,#12193,#12194,#12195,#12196,
#12197,#12198,#12199,#12200,#12201,#12202,#12203,#12204,#12205,#12206,#12207,
#12208,#12209,#12210,#12211,#12212,#12213,#12214,#12215,#12216,#12217,#12218,
#12219,#12220,#12221,#12222,#12223,#12224,#12225,#12226,#12227),(#12228,
#12229,#12230,#12231,#12232,#12233,#12234,#12235,#12236,#12237,#12238,#12239,
#12240,#12241,#12242,#12243,#12244,#12245,#12246,#12247,#12248,#12249,#12250,
#12251,#12252,#12253,#12254,#12255,#12256,#12257,#12258,#12259,#12260,#12261,
#12262,#12263,#12264,#12265,#12266,#12267,#12268),(#12269,#12270,#12271,
#12272,#12273,#12274,#12275,#12276,#12277,#12278,#12279,#12280,#12281,#12282,
#12283,#12284,#12285,#12286,#12287,#12288,#12289,#12290,#12291,#12292,#12293,
#12294,#12295,#12296,#12297,#12298,#12299,#12300,#12301,#12302,#12303,#12304,
#12305,#12306,#12307,#12308,#12309),(#12310,#12311,#12312,#12313,#12314,
#12315,#12316,#12317,#12318,#12319,#12320,#12321,#12322,#12323,#12324,#12325,
#12326,#12327,#12328,#12329,#12330,#12331,#12332,#12333,#12334,#12335,#12336,
#12337,#12338,#12339,#12340,#12341,#12342,#12343,#12344,#12345,#12346,#12347,
#12348,#12349,#12350),(#12351,#12352,#12353,#12354,#12355,#12356,#12357,
#12358,#12359,#12360,#12361,#12362,#12363,#12364,#12365,#12366,#12367,#12368,
#12369,#12370,#12371,#12372,#12373,#12374,#12375,#12376,#12377,#12378,#12379,
#12380,#12381,#12382,#12383,#12384,#12385,#12386,#12387,#12388,#12389,#12390,
#12391),(#12392,#12393,#12394,#12395,#12396,#12397,#12398,#12399,#12400,
#12401,#12402,#12403,#12404,#12405,#12406,#12407,#12408,#12409,#12410,#12411,
#12412,#12413,#12414,#12415,#12416,#12417,#12418,#12419,#12420,#12421,#12422,
#12423,#12424,#12425,#12426,#12427,#12428,#12429,#12430,#12431,#12432),
(#12433,#12434,#12435,#12436,#12437,#12438,#12439,#12440,#12441,#12442,
#12443,#12444,#12445,#12446,#12447,#12448,#12449,#12450,#12451,#12452,#12453,
#12454,#12455,#12456,#12457,#12458,#12459,#12460,#12461,#12462,#12463,#12464,
#12465,#12466,#12467,#12468,#12469,#12470,#12471,#12472,#12473)),
 .UNSPECIFIED.,.T.,.F.,.F.,(4,1,1,1,1,1,1,4),(4,1,1,1,1,1,1,1,1,1,1,1,1,
1,1,1,1,1,1,1,1,1,1,1,1,1,1,1,1,1,1,1,1,1,1,1,1,1,4),(-3.14159265358979,
-2.24399475256414,-1.34639685153848,-0.448798950512828,0.448798950512828,
1.34639685153848,2.24399475256414,3.14159265358979),(0.,0.0357142857142857,
0.0714285714285714,0.107142857142857,0.142857142857143,0.182539682539683,
0.19047619047619,0.214285714285714,0.238095238095238,0.261904761904762,
0.285714285714286,0.30952380952381,0.333333333333333,0.357142857142857,
0.380952380952381,0.412698412698413,0.420634920634921,0.428571428571429,
0.452380952380952,0.476190476190476,0.5,0.535714285714286,0.571428571428571,
0.607142857142857,0.642857142857143,0.678571428571428,0.696428571428571,
0.714285714285714,0.738095238095238,0.761904761904762,0.785714285714286,
0.809523809523809,0.833333333333333,0.857142857142857,0.875,0.892857142857143,
0.928571428571429,0.964285714285714,1.),.UNSPECIFIED.);
#498=B_SPLINE_CURVE_WITH_KNOTS('',3,(#11959,#11960,#11961,#11962,#11963,
#11964,#11965,#11966,#11967,#11968,#11969,#11970,#11971,#11972,#11973,#11974),
 .UNSPECIFIED.,.F.,.F.,(4,2,2,2,2,2,2,4),(-0.118162253960396,-0.11336417636029,
-0.0958062481624726,-0.0759366794145766,-0.0500215343183712,-0.0256788879713264,
0.,0.000489721640252749),.UNSPECIFIED.);
#499=B_SPLINE_CURVE_WITH_KNOTS('',3,(#11976,#11977,#11978,#11979,#11980,
#11981,#11982,#11983,#11984,#11985,#11986,#11987),.UNSPECIFIED.,.F.,.F.,
(4,2,2,2,2,4),(-0.218927972079618,-0.218528918486379,-0.18233291161771,
-0.153633681230302,-0.131619262867663,-0.118162253960396),.UNSPECIFIED.);
#500=B_SPLINE_CURVE_WITH_KNOTS('',3,(#12000,#12001,#12002,#12003,#12004,
#12005,#12006,#12007,#12008,#12009,#12010,#12011,#12012,#12013,#12014,#12015,
#12016,#12017,#12018,#12019,#12020,#12021,#12022,#12023,#12024,#12025,#12026,
#12027,#12028,#12029,#12030,#12031,#12032,#12033,#12034,#12035,#12036,#12037),
 .UNSPECIFIED.,.F.,.F.,(4,2,2,2,2,2,2,2,2,2,2,2,2,2,2,2,2,2,4),(-1.13171649654428,
-1.12635701987523,-0.945490005864125,-0.858292232112738,-0.829544128659967,
-0.817491257372727,-0.809719894883687,-0.801050781771893,-0.788842647214847,
-0.75932496601718,-0.695869882146734,-0.544122263235791,-0.475791925078994,
-0.456893383447211,-0.445776710112588,-0.436652368911013,-0.42698245595475,
-0.412387973442962,-0.410759286941866),.UNSPECIFIED.);
#501=B_SPLINE_CURVE_WITH_KNOTS('',3,(#12041,#12042,#12043,#12044,#12045,
#12046,#12047,#12048,#12049,#12050),.UNSPECIFIED.,.F.,.F.,(4,2,2,2,4),(-0.250413310593431,
-0.210654522228088,-0.0946898181455716,0.,0.00262144099416576),
 .UNSPECIFIED.);
#502=B_SPLINE_CURVE_WITH_KNOTS('',3,(#12051,#12052,#12053,#12054,#12055,
#12056,#12057,#12058),.UNSPECIFIED.,.F.,.F.,(4,2,2,4),(-0.410759286941866,
-0.382265373853863,-0.310503261016197,-0.250413310593431),.UNSPECIFIED.);
#503=B_SPLINE_CURVE_WITH_KNOTS('',3,(#12474,#12475,#12476,#12477,#12478,
#12479,#12480,#12481,#12482,#12483,#12484,#12485,#12486,#12487,#12488,#12489,
#12490,#12491,#12492,#12493,#12494,#12495,#12496,#12497,#12498,#12499,#12500,
#12501,#12502,#12503,#12504,#12505,#12506,#12507,#12508,#12509,#12510,#12511,
#12512,#12513,#12514,#12515,#12516,#12517,#12518,#12519,#12520,#12521,#12522,
#12523,#12524,#12525,#12526,#12527,#12528,#12529,#12530,#12531,#12532,#12533,
#12534,#12535,#12536,#12537,#12538,#12539,#12540,#12541,#12542,#12543,#12544,
#12545,#12546,#12547,#12548,#12549,#12550,#12551,#12552,#12553,#12554,#12555,
#12556,#12557,#12558,#12559,#12560,#12561,#12562,#12563,#12564,#12565,#12566,
#12567,#12568,#12569,#12570,#12571,#12572,#12573,#12574,#12575,#12576,#12577,
#12578,#12579,#12580,#12581,#12582,#12583,#12584,#12585,#12586,#12587,#12588),
 .UNSPECIFIED.,.F.,.F.,(4,3,3,3,3,3,3,3,3,3,3,3,3,3,3,3,3,3,3,3,3,3,3,3,
3,3,3,3,3,3,3,3,3,3,3,3,3,3,4),(0.0181496364157079,0.035714285714264,0.0714285714285062,
0.107142857142748,0.142857142856991,0.182539682539482,0.19047619047598,
0.214285714285475,0.23809523809497,0.261904761904465,0.28571428571396,0.309523809523454,
0.333333333332949,0.357142857142444,0.380952380951939,0.412698412697932,
0.42063492063443,0.428571428570928,0.452380952380423,0.476190476189918,
0.499999999999413,0.535714285713655,0.571428571427897,0.607142857142139,
0.642857142856382,0.678571428570624,0.696428571427745,0.714285714284866,
0.738095238094361,0.761904761903856,0.785714285713351,0.809523809522845,
0.83333333333234,0.857142857141835,0.874999999998956,0.892857142856077,
0.92857142857032,0.964285714284562,0.99631830509798),.UNSPECIFIED.);
#504=B_SPLINE_CURVE_WITH_KNOTS('',3,(#13344,#13345,#13346,#13347,#13348,
#13349,#13350,#13351,#13352,#13353,#13354,#13355,#13356,#13357,#13358,#13359,
#13360,#13361,#13362,#13363,#13364,#13365),.UNSPECIFIED.,.F.,.F.,(4,2,2,
2,2,2,2,2,2,2,4),(0.0473477652366656,0.126350602536658,0.189525903804987,
0.252701205073317,0.313298422430275,0.373895639787233,0.434492857144191,
0.495090074501149,0.558265375769478,0.621440677037807,0.7004435143378),
 .UNSPECIFIED.);
#505=B_SPLINE_CURVE_WITH_KNOTS('',3,(#13369,#13370,#13371,#13372,#13373,
#13374,#13375,#13376,#13377,#13378,#13379,#13380,#13381,#13382,#13383,#13384,
#13385,#13386,#13387,#13388,#13389,#13390),.UNSPECIFIED.,.F.,.F.,(4,2,2,
2,2,2,2,2,2,2,4),(0.0464897534940957,0.0852567806515119,0.170513561303024,
0.246687263103517,0.308657850341199,0.370628437578881,0.432599024816563,
0.494569612054245,0.570743313854739,0.656000094506251,0.694767121663666),
 .UNSPECIFIED.);
#506=B_SPLINE_CURVE_WITH_KNOTS('',3,(#13396,#13397,#13398,#13399,#13400,
#13401,#13402,#13403,#13404,#13405,#13406,#13407,#13408,#13409,#13410,#13411,
#13412,#13413,#13414,#13415,#13416,#13417),.UNSPECIFIED.,.F.,.F.,(4,2,2,
2,2,2,2,2,2,2,4),(0.0464897534940957,0.0852567806515118,0.170513561303024,
0.246687263103517,0.308657850341199,0.370628437578881,0.432599024816563,
0.494569612054245,0.570743313854738,0.65600009450625,0.694767121663666),
 .UNSPECIFIED.);
#507=B_SPLINE_CURVE_WITH_KNOTS('',3,(#13421,#13422,#13423,#13424,#13425,
#13426,#13427,#13428,#13429,#13430,#13431,#13432,#13433,#13434,#13435,#13436,
#13437,#13438,#13439,#13440,#13441,#13442),.UNSPECIFIED.,.F.,.F.,(4,2,2,
2,2,2,2,2,2,2,4),(0.0464897534940957,0.0852567806515119,0.170513561303024,
0.246687263103517,0.308657850341199,0.370628437578881,0.432599024816563,
0.494569612054245,0.570743313854739,0.656000094506251,0.694767121663666),
 .UNSPECIFIED.);
#508=B_SPLINE_CURVE_WITH_KNOTS('',3,(#13446,#13447,#13448,#13449,#13450,
#13451,#13452,#13453,#13454,#13455,#13456,#13457),.UNSPECIFIED.,.F.,.F.,
(4,2,2,2,2,4),(0.0464897534940957,0.0852567806515119,0.170513561303024,
0.246687263103517,0.308657850341199,0.370628437578881),.UNSPECIFIED.);
#509=B_SPLINE_CURVE_WITH_KNOTS('',3,(#13462,#13463,#13464,#13465,#13466,
#13467,#13468,#13469,#13470,#13471,#13472,#13473),.UNSPECIFIED.,.F.,.F.,
(4,2,2,2,2,4),(0.370628437578881,0.432599024816563,0.494569612054245,0.570743313854738,
0.65600009450625,0.694767121663666),.UNSPECIFIED.);
#510=B_SPLINE_CURVE_WITH_KNOTS('',3,(#13477,#13478,#13479,#13480,#13481,
#13482,#13483,#13484,#13485,#13486,#13487,#13488,#13489,#13490,#13491,#13492,
#13493,#13494,#13495,#13496,#13497,#13498),.UNSPECIFIED.,.F.,.F.,(4,2,2,
2,2,2,2,2,2,2,4),(0.0464897534940957,0.0852567806515121,0.170513561303024,
0.246687263103518,0.308657850341199,0.370628437578881,0.432599024816563,
0.494569612054245,0.570743313854738,0.65600009450625,0.694767121663666),
 .UNSPECIFIED.);
#511=B_SPLINE_CURVE_WITH_KNOTS('',3,(#13502,#13503,#13504,#13505,#13506,
#13507,#13508,#13509,#13510,#13511,#13512,#13513,#13514,#13515,#13516,#13517,
#13518,#13519,#13520,#13521,#13522,#13523),.UNSPECIFIED.,.F.,.F.,(4,2,2,
2,2,2,2,2,2,2,4),(0.0464897534940957,0.0852567806515119,0.170513561303024,
0.246687263103517,0.308657850341199,0.370628437578881,0.432599024816563,
0.494569612054245,0.570743313854738,0.65600009450625,0.694767121663667),
 .UNSPECIFIED.);
#512=B_SPLINE_CURVE_WITH_KNOTS('',3,(#13527,#13528,#13529,#13530,#13531,
#13532,#13533,#13534,#13535,#13536,#13537,#13538,#13539,#13540,#13541,#13542,
#13543,#13544,#13545,#13546,#13547,#13548),.UNSPECIFIED.,.F.,.F.,(4,2,2,
2,2,2,2,2,2,2,4),(0.0464897534940957,0.0852567806515119,0.170513561303024,
0.246687263103517,0.308657850341199,0.370628437578881,0.432599024816563,
0.494569612054245,0.570743313854738,0.65600009450625,0.694767121663666),
 .UNSPECIFIED.);
#513=B_SPLINE_CURVE_WITH_KNOTS('',3,(#13552,#13553,#13554,#13555,#13556,
#13557,#13558,#13559,#13560,#13561,#13562,#13563,#13564,#13565,#13566,#13567,
#13568,#13569,#13570,#13571,#13572,#13573),.UNSPECIFIED.,.F.,.F.,(4,2,2,
2,2,2,2,2,2,2,4),(0.0464897534940957,0.0852567806515119,0.170513561303024,
0.246687263103517,0.308657850341199,0.370628437578881,0.432599024816563,
0.494569612054245,0.570743313854739,0.656000094506251,0.694767121663667),
 .UNSPECIFIED.);
#514=B_SPLINE_CURVE_WITH_KNOTS('',3,(#13581,#13582,#13583,#13584,#13585,
#13586,#13587,#13588,#13589,#13590,#13591,#13592,#13593,#13594,#13595,#13596,
#13597,#13598,#13599,#13600,#13601,#13602),.UNSPECIFIED.,.F.,.F.,(4,2,2,
2,2,2,2,2,2,2,4),(0.0473477652366656,0.126350602536658,0.189525903804987,
0.252701205073316,0.313298422430274,0.373895639787232,0.434492857144191,
0.495090074501149,0.558265375769478,0.621440677037807,0.7004435143378),
 .UNSPECIFIED.);
#515=B_SPLINE_CURVE_WITH_KNOTS('',3,(#13610,#13611,#13612,#13613,#13614,
#13615,#13616,#13617,#13618,#13619,#13620,#13621,#13622,#13623,#13624,#13625,
#13626,#13627,#13628,#13629,#13630,#13631),.UNSPECIFIED.,.F.,.F.,(4,2,2,
2,2,2,2,2,2,2,4),(0.0473477652366656,0.126350602536658,0.189525903804987,
0.252701205073317,0.313298422430275,0.373895639787233,0.434492857144191,
0.495090074501149,0.558265375769478,0.621440677037807,0.7004435143378),
 .UNSPECIFIED.);
#516=B_SPLINE_CURVE_WITH_KNOTS('',3,(#13640,#13641,#13642,#13643,#13644,
#13645,#13646,#13647,#13648,#13649,#13650,#13651),.UNSPECIFIED.,.F.,.F.,
(4,2,2,2,2,4),(0.0473477652366656,0.126350602536658,0.189525903804987,0.252701205073316,
0.313298422430275,0.373895639787233),.UNSPECIFIED.);
#517=B_SPLINE_CURVE_WITH_KNOTS('',3,(#13653,#13654,#13655,#13656,#13657,
#13658,#13659,#13660,#13661,#13662,#13663,#13664),.UNSPECIFIED.,.F.,.F.,
(4,2,2,2,2,4),(0.373895639787233,0.434492857144191,0.495090074501149,0.558265375769478,
0.621440677037807,0.7004435143378),.UNSPECIFIED.);
#518=B_SPLINE_CURVE_WITH_KNOTS('',3,(#13671,#13672,#13673,#13674,#13675,
#13676,#13677,#13678,#13679,#13680,#13681,#13682,#13683,#13684,#13685,#13686,
#13687,#13688,#13689,#13690,#13691,#13692),.UNSPECIFIED.,.F.,.F.,(4,2,2,
2,2,2,2,2,2,2,4),(0.0473477652366656,0.126350602536658,0.189525903804987,
0.252701205073316,0.313298422430275,0.373895639787233,0.434492857144191,
0.495090074501149,0.558265375769478,0.621440677037807,0.7004435143378),
 .UNSPECIFIED.);
#519=B_SPLINE_CURVE_WITH_KNOTS('',3,(#13700,#13701,#13702,#13703,#13704,
#13705,#13706,#13707,#13708,#13709,#13710,#13711,#13712,#13713,#13714,#13715,
#13716,#13717,#13718,#13719,#13720,#13721),.UNSPECIFIED.,.F.,.F.,(4,2,2,
2,2,2,2,2,2,2,4),(0.0473477652366656,0.126350602536658,0.189525903804987,
0.252701205073317,0.313298422430275,0.373895639787233,0.434492857144191,
0.495090074501149,0.558265375769478,0.621440677037807,0.7004435143378),
 .UNSPECIFIED.);
#520=B_SPLINE_CURVE_WITH_KNOTS('',3,(#13729,#13730,#13731,#13732,#13733,
#13734,#13735,#13736,#13737,#13738,#13739,#13740,#13741,#13742,#13743,#13744,
#13745,#13746,#13747,#13748,#13749,#13750),.UNSPECIFIED.,.F.,.F.,(4,2,2,
2,2,2,2,2,2,2,4),(0.0473477652366656,0.126350602536658,0.189525903804987,
0.252701205073316,0.313298422430275,0.373895639787233,0.434492857144191,
0.495090074501149,0.558265375769478,0.621440677037807,0.7004435143378),
 .UNSPECIFIED.);
#521=B_SPLINE_CURVE_WITH_KNOTS('',3,(#13759,#13760,#13761,#13762,#13763,
#13764,#13765,#13766,#13767,#13768,#13769,#13770,#13771,#13772,#13773,#13774,
#13775,#13776,#13777,#13778,#13779,#13780),.UNSPECIFIED.,.F.,.F.,(4,2,2,
2,2,2,2,2,2,2,4),(0.0473477652366656,0.126350602536658,0.189525903804987,
0.252701205073317,0.313298422430275,0.373895639787233,0.434492857144191,
0.495090074501149,0.558265375769478,0.621440677037807,0.7004435143378),
 .UNSPECIFIED.);
#522=SHAPE_REPRESENTATION_RELATIONSHIP('SRR','None',#14743,#572);
#523=SHAPE_REPRESENTATION_RELATIONSHIP('SRR','None',#14744,#573);
#524=SHAPE_REPRESENTATION_RELATIONSHIP('SRR','None',#14745,#574);
#525=SHAPE_REPRESENTATION_RELATIONSHIP('SRR','None',#14746,#575);
#526=SHAPE_REPRESENTATION_RELATIONSHIP('SRR','None',#14747,#576);
#527=SHAPE_REPRESENTATION_RELATIONSHIP('SRR','None',#14748,#577);
#528=SHAPE_REPRESENTATION_RELATIONSHIP('SRR','None',#14749,#578);
#529=SHAPE_REPRESENTATION_RELATIONSHIP('SRR','None',#14750,#579);
#530=SHAPE_REPRESENTATION_RELATIONSHIP('SRR','None',#14751,#580);
#531=SHAPE_REPRESENTATION_RELATIONSHIP('SRR','None',#14752,#581);
#532=SHAPE_REPRESENTATION_RELATIONSHIP('SRR','None',#14753,#582);
#533=SHAPE_REPRESENTATION_RELATIONSHIP('SRR','None',#14754,#583);
#534=SHAPE_REPRESENTATION_RELATIONSHIP('SRR','None',#14755,#584);
#535=SHAPE_REPRESENTATION_RELATIONSHIP('SRR','None',#14756,#585);
#536=SHAPE_REPRESENTATION_RELATIONSHIP('SRR','None',#14757,#586);
#537=SHAPE_REPRESENTATION_RELATIONSHIP('SRR','None',#14758,#587);
#538=SHAPE_REPRESENTATION_RELATIONSHIP('SRR','None',#14759,#588);
#539=SHAPE_REPRESENTATION_RELATIONSHIP('SRR','None',#14761,#589);
#540=SHAPE_REPRESENTATION_RELATIONSHIP('SRR','None',#14762,#590);
#541=SHAPE_REPRESENTATION_RELATIONSHIP('SRR','None',#14763,#591);
#542=SHAPE_REPRESENTATION_RELATIONSHIP('SRR','None',#14764,#592);
#543=SHAPE_REPRESENTATION_RELATIONSHIP('SRR','None',#14765,#593);
#544=SHAPE_REPRESENTATION_RELATIONSHIP('SRR','None',#14766,#594);
#545=SHAPE_REPRESENTATION_RELATIONSHIP('SRR','None',#14767,#595);
#546=SHAPE_REPRESENTATION_RELATIONSHIP('SRR','None',#14768,#596);
#547=SHAPE_REPRESENTATION_RELATIONSHIP('SRR','None',#14770,#597);
#548=SHAPE_REPRESENTATION_RELATIONSHIP('SRR','None',#14771,#598);
#549=SHAPE_REPRESENTATION_RELATIONSHIP('SRR','None',#14772,#599);
#550=SHAPE_REPRESENTATION_RELATIONSHIP('SRR','None',#14773,#600);
#551=SHAPE_REPRESENTATION_RELATIONSHIP('SRR','None',#14774,#601);
#552=SHAPE_REPRESENTATION_RELATIONSHIP('SRR','None',#14775,#602);
#553=SHAPE_REPRESENTATION_RELATIONSHIP('SRR','None',#14776,#603);
#554=SHAPE_REPRESENTATION_RELATIONSHIP('SRR','None',#14778,#604);
#555=SHAPE_REPRESENTATION_RELATIONSHIP('SRR','None',#14779,#605);
#556=SHAPE_REPRESENTATION_RELATIONSHIP('SRR','None',#14780,#606);
#557=SHAPE_REPRESENTATION_RELATIONSHIP('SRR','None',#14781,#607);
#558=SHAPE_REPRESENTATION_RELATIONSHIP('SRR','None',#14782,#608);
#559=SHAPE_REPRESENTATION_RELATIONSHIP('SRR','None',#14783,#609);
#560=SHAPE_REPRESENTATION_RELATIONSHIP('SRR','None',#14785,#610);
#561=SHAPE_REPRESENTATION_RELATIONSHIP('SRR','None',#14786,#611);
#562=SHAPE_REPRESENTATION_RELATIONSHIP('SRR','None',#14787,#612);
#563=SHAPE_REPRESENTATION_RELATIONSHIP('SRR','None',#14788,#613);
#564=SHAPE_REPRESENTATION_RELATIONSHIP('SRR','None',#14789,#614);
#565=SHAPE_REPRESENTATION_RELATIONSHIP('SRR','None',#14790,#615);
#566=SHAPE_REPRESENTATION_RELATIONSHIP('SRR','None',#14791,#616);
#567=SHAPE_REPRESENTATION_RELATIONSHIP('SRR','None',#14792,#617);
#568=SHAPE_REPRESENTATION_RELATIONSHIP('SRR','None',#14793,#618);
#569=SHAPE_REPRESENTATION_RELATIONSHIP('SRR','None',#14794,#619);
#570=SHAPE_REPRESENTATION_RELATIONSHIP('SRR','None',#14795,#620);
#571=SHAPE_REPRESENTATION_RELATIONSHIP('SRR','None',#14796,#621);
#572=ADVANCED_BREP_SHAPE_REPRESENTATION('',(#680),#14458);
#573=ADVANCED_BREP_SHAPE_REPRESENTATION('',(#681),#14459);
#574=ADVANCED_BREP_SHAPE_REPRESENTATION('',(#682),#14460);
#575=ADVANCED_BREP_SHAPE_REPRESENTATION('',(#683),#14461);
#576=ADVANCED_BREP_SHAPE_REPRESENTATION('',(#684),#14462);
#577=ADVANCED_BREP_SHAPE_REPRESENTATION('',(#685),#14463);
#578=ADVANCED_BREP_SHAPE_REPRESENTATION('',(#686),#14464);
#579=ADVANCED_BREP_SHAPE_REPRESENTATION('',(#687),#14465);
#580=ADVANCED_BREP_SHAPE_REPRESENTATION('',(#688),#14466);
#581=ADVANCED_BREP_SHAPE_REPRESENTATION('',(#689),#14467);
#582=ADVANCED_BREP_SHAPE_REPRESENTATION('',(#690),#14468);
#583=ADVANCED_BREP_SHAPE_REPRESENTATION('',(#691),#14469);
#584=ADVANCED_BREP_SHAPE_REPRESENTATION('',(#692),#14470);
#585=ADVANCED_BREP_SHAPE_REPRESENTATION('',(#693),#14471);
#586=ADVANCED_BREP_SHAPE_REPRESENTATION('',(#694),#14472);
#587=ADVANCED_BREP_SHAPE_REPRESENTATION('',(#695),#14473);
#588=ADVANCED_BREP_SHAPE_REPRESENTATION('',(#494),#14474);
#589=ADVANCED_BREP_SHAPE_REPRESENTATION('',(#696),#14476);
#590=ADVANCED_BREP_SHAPE_REPRESENTATION('',(#697),#14477);
#591=ADVANCED_BREP_SHAPE_REPRESENTATION('',(#698),#14478);
#592=ADVANCED_BREP_SHAPE_REPRESENTATION('',(#699),#14479);
#593=ADVANCED_BREP_SHAPE_REPRESENTATION('',(#700),#14480);
#594=ADVANCED_BREP_SHAPE_REPRESENTATION('',(#701),#14481);
#595=ADVANCED_BREP_SHAPE_REPRESENTATION('',(#702),#14482);
#596=ADVANCED_BREP_SHAPE_REPRESENTATION('',(#703),#14483);
#597=ADVANCED_BREP_SHAPE_REPRESENTATION('',(#704),#14485);
#598=ADVANCED_BREP_SHAPE_REPRESENTATION('',(#705),#14486);
#599=ADVANCED_BREP_SHAPE_REPRESENTATION('',(#706),#14487);
#600=ADVANCED_BREP_SHAPE_REPRESENTATION('',(#707),#14488);
#601=ADVANCED_BREP_SHAPE_REPRESENTATION('',(#708),#14489);
#602=ADVANCED_BREP_SHAPE_REPRESENTATION('',(#709),#14490);
#603=ADVANCED_BREP_SHAPE_REPRESENTATION('',(#710),#14491);
#604=ADVANCED_BREP_SHAPE_REPRESENTATION('',(#711),#14493);
#605=ADVANCED_BREP_SHAPE_REPRESENTATION('',(#712),#14494);
#606=ADVANCED_BREP_SHAPE_REPRESENTATION('',(#713,#714,#715,#716,#717,#718,
#719,#720),#14495);
#607=ADVANCED_BREP_SHAPE_REPRESENTATION('',(#721),#14496);
#608=ADVANCED_BREP_SHAPE_REPRESENTATION('',(#722,#723),#14497);
#609=ADVANCED_BREP_SHAPE_REPRESENTATION('',(#495),#14498);
#610=ADVANCED_BREP_SHAPE_REPRESENTATION('',(#724),#14500);
#611=ADVANCED_BREP_SHAPE_REPRESENTATION('',(#725),#14501);
#612=ADVANCED_BREP_SHAPE_REPRESENTATION('',(#726),#14502);
#613=ADVANCED_BREP_SHAPE_REPRESENTATION('',(#727),#14503);
#614=ADVANCED_BREP_SHAPE_REPRESENTATION('',(#728),#14504);
#615=ADVANCED_BREP_SHAPE_REPRESENTATION('',(#729),#14505);
#616=ADVANCED_BREP_SHAPE_REPRESENTATION('',(#730),#14506);
#617=ADVANCED_BREP_SHAPE_REPRESENTATION('',(#731),#14507);
#618=ADVANCED_BREP_SHAPE_REPRESENTATION('',(#732),#14508);
#619=ADVANCED_BREP_SHAPE_REPRESENTATION('',(#733),#14509);
#620=ADVANCED_BREP_SHAPE_REPRESENTATION('',(#734),#14510);
#621=ADVANCED_BREP_SHAPE_REPRESENTATION('',(#496),#14511);
#622=STYLED_ITEM('',(#15066),#680);
#623=STYLED_ITEM('',(#15073),#681);
#624=STYLED_ITEM('',(#15073),#682);
#625=STYLED_ITEM('',(#15101),#683);
#626=STYLED_ITEM('',(#15087),#684);
#627=STYLED_ITEM('',(#15087),#685);
#628=STYLED_ITEM('',(#15080),#686);
#629=STYLED_ITEM('',(#15073),#687);
#630=STYLED_ITEM('',(#15101),#688);
#631=STYLED_ITEM('',(#15087),#689);
#632=STYLED_ITEM('',(#15087),#690);
#633=STYLED_ITEM('',(#15080),#691);
#634=STYLED_ITEM('',(#15080),#692);
#635=STYLED_ITEM('',(#15101),#693);
#636=STYLED_ITEM('',(#15087),#694);
#637=STYLED_ITEM('',(#15087),#695);
#638=STYLED_ITEM('',(#15094),#494);
#639=STYLED_ITEM('',(#15101),#696);
#640=STYLED_ITEM('',(#15087),#697);
#641=STYLED_ITEM('',(#15087),#698);
#642=STYLED_ITEM('',(#15087),#699);
#643=STYLED_ITEM('',(#15087),#700);
#644=STYLED_ITEM('',(#15087),#701);
#645=STYLED_ITEM('',(#15087),#702);
#646=STYLED_ITEM('',(#15087),#703);
#647=STYLED_ITEM('',(#15101),#704);
#648=STYLED_ITEM('',(#15087),#705);
#649=STYLED_ITEM('',(#15087),#706);
#650=STYLED_ITEM('',(#15087),#707);
#651=STYLED_ITEM('',(#15087),#708);
#652=STYLED_ITEM('',(#15087),#709);
#653=STYLED_ITEM('',(#15087),#710);
#654=STYLED_ITEM('',(#15087),#711);
#655=STYLED_ITEM('',(#15087),#712);
#656=STYLED_ITEM('',(#15087),#713);
#657=STYLED_ITEM('',(#15087),#714);
#658=STYLED_ITEM('',(#15087),#715);
#659=STYLED_ITEM('',(#15087),#716);
#660=STYLED_ITEM('',(#15087),#717);
#661=STYLED_ITEM('',(#15087),#718);
#662=STYLED_ITEM('',(#15087),#719);
#663=STYLED_ITEM('',(#15087),#720);
#664=STYLED_ITEM('',(#15087),#721);
#665=STYLED_ITEM('',(#15087),#722);
#666=STYLED_ITEM('',(#15087),#723);
#667=STYLED_ITEM('',(#15094),#495);
#668=STYLED_ITEM('',(#15080),#724);
#669=STYLED_ITEM('',(#15087),#725);
#670=STYLED_ITEM('',(#15087),#726);
#671=STYLED_ITEM('',(#15080),#727);
#672=STYLED_ITEM('',(#15080),#728);
#673=STYLED_ITEM('',(#15101),#729);
#674=STYLED_ITEM('',(#15087),#730);
#675=STYLED_ITEM('',(#15087),#731);
#676=STYLED_ITEM('',(#15080),#732);
#677=STYLED_ITEM('',(#15080),#733);
#678=STYLED_ITEM('',(#15101),#734);
#679=STYLED_ITEM('',(#15094),#496);
#680=MANIFOLD_SOLID_BREP('Body1',#7326);
#681=MANIFOLD_SOLID_BREP('Body1',#7327);
#682=MANIFOLD_SOLID_BREP('Body1',#7328);
#683=MANIFOLD_SOLID_BREP('Body1',#7329);
#684=MANIFOLD_SOLID_BREP('Body1',#7330);
#685=MANIFOLD_SOLID_BREP('Body1',#7331);
#686=MANIFOLD_SOLID_BREP('Body1',#7332);
#687=MANIFOLD_SOLID_BREP('Body1',#7333);
#688=MANIFOLD_SOLID_BREP('Body1',#7334);
#689=MANIFOLD_SOLID_BREP('Body1',#7335);
#690=MANIFOLD_SOLID_BREP('Body1',#7336);
#691=MANIFOLD_SOLID_BREP('Body1',#7337);
#692=MANIFOLD_SOLID_BREP('Body1',#7338);
#693=MANIFOLD_SOLID_BREP('Body1',#7339);
#694=MANIFOLD_SOLID_BREP('Body1',#7340);
#695=MANIFOLD_SOLID_BREP('Body1',#7341);
#696=MANIFOLD_SOLID_BREP('Body1',#7344);
#697=MANIFOLD_SOLID_BREP('Body1',#7345);
#698=MANIFOLD_SOLID_BREP('Body1',#7346);
#699=MANIFOLD_SOLID_BREP('Body1',#7347);
#700=MANIFOLD_SOLID_BREP('Body1',#7348);
#701=MANIFOLD_SOLID_BREP('Body1',#7349);
#702=MANIFOLD_SOLID_BREP('Body1',#7350);
#703=MANIFOLD_SOLID_BREP('Body1',#7351);
#704=MANIFOLD_SOLID_BREP('Body1',#7352);
#705=MANIFOLD_SOLID_BREP('Body1',#7353);
#706=MANIFOLD_SOLID_BREP('Body1',#7354);
#707=MANIFOLD_SOLID_BREP('Body1',#7355);
#708=MANIFOLD_SOLID_BREP('Body1',#7356);
#709=MANIFOLD_SOLID_BREP('Body1',#7357);
#710=MANIFOLD_SOLID_BREP('Body1',#7358);
#711=MANIFOLD_SOLID_BREP('Body1',#7359);
#712=MANIFOLD_SOLID_BREP('Body1',#7360);
#713=MANIFOLD_SOLID_BREP('Body1',#7361);
#714=MANIFOLD_SOLID_BREP('Body2',#7362);
#715=MANIFOLD_SOLID_BREP('Body3',#7363);
#716=MANIFOLD_SOLID_BREP('Body4',#7364);
#717=MANIFOLD_SOLID_BREP('Body5',#7365);
#718=MANIFOLD_SOLID_BREP('Body6',#7366);
#719=MANIFOLD_SOLID_BREP('Body7',#7367);
#720=MANIFOLD_SOLID_BREP('Body8',#7368);
#721=MANIFOLD_SOLID_BREP('Continuous crown cage',#7369);
#722=MANIFOLD_SOLID_BREP('Body1',#7370);
#723=MANIFOLD_SOLID_BREP('Body2',#7371);
#724=MANIFOLD_SOLID_BREP('Body1',#7374);
#725=MANIFOLD_SOLID_BREP('Body1',#7375);
#726=MANIFOLD_SOLID_BREP('Body1',#7376);
#727=MANIFOLD_SOLID_BREP('Body1',#7377);
#728=MANIFOLD_SOLID_BREP('Body1',#7378);
#729=MANIFOLD_SOLID_BREP('Body1',#7379);
#730=MANIFOLD_SOLID_BREP('Body1',#7380);
#731=MANIFOLD_SOLID_BREP('Body1',#7381);
#732=MANIFOLD_SOLID_BREP('Body1',#7382);
#733=MANIFOLD_SOLID_BREP('Body1',#7383);
#734=MANIFOLD_SOLID_BREP('Body1',#7384);
#735=FACE_BOUND('',#1630,.T.);
#736=FACE_BOUND('',#1631,.T.);
#737=FACE_BOUND('',#1632,.T.);
#738=FACE_BOUND('',#1633,.T.);
#739=FACE_BOUND('',#1635,.T.);
#740=FACE_BOUND('',#1636,.T.);
#741=FACE_BOUND('',#1637,.T.);
#742=FACE_BOUND('',#1638,.T.);
#743=FACE_BOUND('',#1666,.T.);
#744=FACE_BOUND('',#1667,.T.);
#745=FACE_BOUND('',#1668,.T.);
#746=FACE_BOUND('',#1669,.T.);
#747=FACE_BOUND('',#1672,.T.);
#748=FACE_BOUND('',#1673,.T.);
#749=FACE_BOUND('',#1674,.T.);
#750=FACE_BOUND('',#1675,.T.);
#751=FACE_BOUND('',#1679,.T.);
#752=FACE_BOUND('',#1680,.T.);
#753=FACE_BOUND('',#1681,.T.);
#754=FACE_BOUND('',#1682,.T.);
#755=FACE_BOUND('',#1683,.T.);
#756=FACE_BOUND('',#1684,.T.);
#757=FACE_BOUND('',#1685,.T.);
#758=FACE_BOUND('',#1686,.T.);
#759=FACE_BOUND('',#1689,.T.);
#760=FACE_BOUND('',#1690,.T.);
#761=FACE_BOUND('',#1691,.T.);
#762=FACE_BOUND('',#1692,.T.);
#763=FACE_BOUND('',#1693,.T.);
#764=FACE_BOUND('',#1694,.T.);
#765=FACE_BOUND('',#1695,.T.);
#766=FACE_BOUND('',#1696,.T.);
#767=FACE_BOUND('',#1698,.T.);
#768=FACE_BOUND('',#1706,.T.);
#769=FACE_BOUND('',#1707,.T.);
#770=FACE_BOUND('',#1708,.T.);
#771=FACE_BOUND('',#1709,.T.);
#772=FACE_BOUND('',#1711,.T.);
#773=FACE_BOUND('',#1712,.T.);
#774=FACE_BOUND('',#1713,.T.);
#775=FACE_BOUND('',#1714,.T.);
#776=FACE_BOUND('',#1720,.T.);
#777=FACE_BOUND('',#1724,.T.);
#778=FACE_BOUND('',#1726,.T.);
#779=FACE_BOUND('',#1730,.T.);
#780=FACE_BOUND('',#1732,.T.);
#781=FACE_BOUND('',#1736,.T.);
#782=FACE_BOUND('',#1738,.T.);
#783=FACE_BOUND('',#1742,.T.);
#784=FACE_BOUND('',#1744,.T.);
#785=FACE_BOUND('',#1751,.T.);
#786=FACE_BOUND('',#1752,.T.);
#787=FACE_BOUND('',#1753,.T.);
#788=FACE_BOUND('',#1754,.T.);
#789=FACE_BOUND('',#1756,.T.);
#790=FACE_BOUND('',#1757,.T.);
#791=FACE_BOUND('',#1758,.T.);
#792=FACE_BOUND('',#1759,.T.);
#793=FACE_BOUND('',#1765,.T.);
#794=FACE_BOUND('',#1769,.T.);
#795=FACE_BOUND('',#1771,.T.);
#796=FACE_BOUND('',#1775,.T.);
#797=FACE_BOUND('',#1777,.T.);
#798=FACE_BOUND('',#1781,.T.);
#799=FACE_BOUND('',#1783,.T.);
#800=FACE_BOUND('',#1787,.T.);
#801=FACE_BOUND('',#1789,.T.);
#802=FACE_BOUND('',#1794,.T.);
#803=FACE_BOUND('',#1800,.T.);
#804=FACE_BOUND('',#1803,.T.);
#805=FACE_BOUND('',#1806,.T.);
#806=FACE_BOUND('',#1830,.T.);
#807=FACE_BOUND('',#1846,.T.);
#808=FACE_BOUND('',#1847,.T.);
#809=FACE_BOUND('',#1848,.T.);
#810=FACE_BOUND('',#1849,.T.);
#811=FACE_BOUND('',#1850,.T.);
#812=FACE_BOUND('',#1851,.T.);
#813=FACE_BOUND('',#1852,.T.);
#814=FACE_BOUND('',#1853,.T.);
#815=FACE_BOUND('',#1854,.T.);
#816=FACE_BOUND('',#1855,.T.);
#817=FACE_BOUND('',#1859,.T.);
#818=FACE_BOUND('',#1860,.T.);
#819=FACE_BOUND('',#1861,.T.);
#820=FACE_BOUND('',#1862,.T.);
#821=FACE_BOUND('',#1863,.T.);
#822=FACE_BOUND('',#1864,.T.);
#823=FACE_BOUND('',#1865,.T.);
#824=FACE_BOUND('',#1866,.T.);
#825=FACE_BOUND('',#1867,.T.);
#826=FACE_BOUND('',#1868,.T.);
#827=FACE_BOUND('',#1872,.T.);
#828=FACE_BOUND('',#1874,.T.);
#829=FACE_BOUND('',#1882,.T.);
#830=FACE_BOUND('',#1883,.T.);
#831=FACE_BOUND('',#1884,.T.);
#832=FACE_BOUND('',#1885,.T.);
#833=FACE_BOUND('',#1886,.T.);
#834=FACE_BOUND('',#1888,.T.);
#835=FACE_BOUND('',#1889,.T.);
#836=FACE_BOUND('',#1890,.T.);
#837=FACE_BOUND('',#1891,.T.);
#838=FACE_BOUND('',#1892,.T.);
#839=FACE_BOUND('',#1900,.T.);
#840=FACE_BOUND('',#1901,.T.);
#841=FACE_BOUND('',#1902,.T.);
#842=FACE_BOUND('',#1903,.T.);
#843=FACE_BOUND('',#1904,.T.);
#844=FACE_BOUND('',#1906,.T.);
#845=FACE_BOUND('',#1907,.T.);
#846=FACE_BOUND('',#1908,.T.);
#847=FACE_BOUND('',#1909,.T.);
#848=FACE_BOUND('',#1910,.T.);
#849=FACE_BOUND('',#1914,.T.);
#850=FACE_BOUND('',#1916,.T.);
#851=FACE_BOUND('',#1924,.T.);
#852=FACE_BOUND('',#1925,.T.);
#853=FACE_BOUND('',#1926,.T.);
#854=FACE_BOUND('',#1927,.T.);
#855=FACE_BOUND('',#1928,.T.);
#856=FACE_BOUND('',#1930,.T.);
#857=FACE_BOUND('',#1931,.T.);
#858=FACE_BOUND('',#1932,.T.);
#859=FACE_BOUND('',#1933,.T.);
#860=FACE_BOUND('',#1934,.T.);
#861=FACE_BOUND('',#1942,.T.);
#862=FACE_BOUND('',#1943,.T.);
#863=FACE_BOUND('',#1944,.T.);
#864=FACE_BOUND('',#1945,.T.);
#865=FACE_BOUND('',#1946,.T.);
#866=FACE_BOUND('',#1948,.T.);
#867=FACE_BOUND('',#1949,.T.);
#868=FACE_BOUND('',#1950,.T.);
#869=FACE_BOUND('',#1951,.T.);
#870=FACE_BOUND('',#1952,.T.);
#871=FACE_BOUND('',#1956,.T.);
#872=FACE_BOUND('',#1959,.T.);
#873=FACE_BOUND('',#1975,.T.);
#874=FACE_BOUND('',#1976,.T.);
#875=FACE_BOUND('',#1977,.T.);
#876=FACE_BOUND('',#1978,.T.);
#877=FACE_BOUND('',#1979,.T.);
#878=FACE_BOUND('',#1980,.T.);
#879=FACE_BOUND('',#1981,.T.);
#880=FACE_BOUND('',#1982,.T.);
#881=FACE_BOUND('',#1983,.T.);
#882=FACE_BOUND('',#1984,.T.);
#883=FACE_BOUND('',#1988,.T.);
#884=FACE_BOUND('',#1989,.T.);
#885=FACE_BOUND('',#1990,.T.);
#886=FACE_BOUND('',#1991,.T.);
#887=FACE_BOUND('',#1992,.T.);
#888=FACE_BOUND('',#1993,.T.);
#889=FACE_BOUND('',#1994,.T.);
#890=FACE_BOUND('',#1995,.T.);
#891=FACE_BOUND('',#1996,.T.);
#892=FACE_BOUND('',#1997,.T.);
#893=FACE_BOUND('',#2001,.T.);
#894=FACE_BOUND('',#2003,.T.);
#895=FACE_BOUND('',#2011,.T.);
#896=FACE_BOUND('',#2012,.T.);
#897=FACE_BOUND('',#2013,.T.);
#898=FACE_BOUND('',#2014,.T.);
#899=FACE_BOUND('',#2015,.T.);
#900=FACE_BOUND('',#2017,.T.);
#901=FACE_BOUND('',#2018,.T.);
#902=FACE_BOUND('',#2019,.T.);
#903=FACE_BOUND('',#2020,.T.);
#904=FACE_BOUND('',#2021,.T.);
#905=FACE_BOUND('',#2029,.T.);
#906=FACE_BOUND('',#2030,.T.);
#907=FACE_BOUND('',#2031,.T.);
#908=FACE_BOUND('',#2032,.T.);
#909=FACE_BOUND('',#2033,.T.);
#910=FACE_BOUND('',#2035,.T.);
#911=FACE_BOUND('',#2036,.T.);
#912=FACE_BOUND('',#2037,.T.);
#913=FACE_BOUND('',#2038,.T.);
#914=FACE_BOUND('',#2039,.T.);
#915=FACE_BOUND('',#2043,.T.);
#916=FACE_BOUND('',#2045,.T.);
#917=FACE_BOUND('',#2053,.T.);
#918=FACE_BOUND('',#2054,.T.);
#919=FACE_BOUND('',#2055,.T.);
#920=FACE_BOUND('',#2056,.T.);
#921=FACE_BOUND('',#2057,.T.);
#922=FACE_BOUND('',#2059,.T.);
#923=FACE_BOUND('',#2060,.T.);
#924=FACE_BOUND('',#2061,.T.);
#925=FACE_BOUND('',#2062,.T.);
#926=FACE_BOUND('',#2063,.T.);
#927=FACE_BOUND('',#2071,.T.);
#928=FACE_BOUND('',#2072,.T.);
#929=FACE_BOUND('',#2073,.T.);
#930=FACE_BOUND('',#2074,.T.);
#931=FACE_BOUND('',#2075,.T.);
#932=FACE_BOUND('',#2077,.T.);
#933=FACE_BOUND('',#2078,.T.);
#934=FACE_BOUND('',#2079,.T.);
#935=FACE_BOUND('',#2080,.T.);
#936=FACE_BOUND('',#2081,.T.);
#937=FACE_BOUND('',#2087,.T.);
#938=FACE_BOUND('',#2090,.T.);
#939=FACE_BOUND('',#2095,.T.);
#940=FACE_BOUND('',#2100,.T.);
#941=FACE_BOUND('',#2128,.T.);
#942=FACE_BOUND('',#2131,.T.);
#943=FACE_BOUND('',#2134,.T.);
#944=FACE_BOUND('',#2137,.T.);
#945=FACE_BOUND('',#2140,.T.);
#946=FACE_BOUND('',#2156,.T.);
#947=FACE_BOUND('',#2174,.T.);
#948=FACE_BOUND('',#2175,.T.);
#949=FACE_BOUND('',#2176,.T.);
#950=FACE_BOUND('',#2177,.T.);
#951=FACE_BOUND('',#2179,.T.);
#952=FACE_BOUND('',#2180,.T.);
#953=FACE_BOUND('',#2181,.T.);
#954=FACE_BOUND('',#2182,.T.);
#955=FACE_BOUND('',#2184,.T.);
#956=FACE_BOUND('',#2185,.T.);
#957=FACE_BOUND('',#2186,.T.);
#958=FACE_BOUND('',#2187,.T.);
#959=FACE_BOUND('',#2188,.T.);
#960=FACE_BOUND('',#2189,.T.);
#961=FACE_BOUND('',#2190,.T.);
#962=FACE_BOUND('',#2191,.T.);
#963=FACE_BOUND('',#2194,.T.);
#964=FACE_BOUND('',#2195,.T.);
#965=FACE_BOUND('',#2196,.T.);
#966=FACE_BOUND('',#2197,.T.);
#967=FACE_BOUND('',#2198,.T.);
#968=FACE_BOUND('',#2199,.T.);
#969=FACE_BOUND('',#2200,.T.);
#970=FACE_BOUND('',#2201,.T.);
#971=FACE_BOUND('',#2210,.T.);
#972=FACE_BOUND('',#2211,.T.);
#973=FACE_BOUND('',#2212,.T.);
#974=FACE_BOUND('',#2213,.T.);
#975=FACE_BOUND('',#2215,.T.);
#976=FACE_BOUND('',#2216,.T.);
#977=FACE_BOUND('',#2217,.T.);
#978=FACE_BOUND('',#2218,.T.);
#979=FACE_BOUND('',#2224,.T.);
#980=FACE_BOUND('',#2228,.T.);
#981=FACE_BOUND('',#2230,.T.);
#982=FACE_BOUND('',#2234,.T.);
#983=FACE_BOUND('',#2236,.T.);
#984=FACE_BOUND('',#2240,.T.);
#985=FACE_BOUND('',#2242,.T.);
#986=FACE_BOUND('',#2246,.T.);
#987=FACE_BOUND('',#2248,.T.);
#988=FACE_BOUND('',#2255,.T.);
#989=FACE_BOUND('',#2256,.T.);
#990=FACE_BOUND('',#2257,.T.);
#991=FACE_BOUND('',#2258,.T.);
#992=FACE_BOUND('',#2260,.T.);
#993=FACE_BOUND('',#2261,.T.);
#994=FACE_BOUND('',#2262,.T.);
#995=FACE_BOUND('',#2263,.T.);
#996=FACE_BOUND('',#2269,.T.);
#997=FACE_BOUND('',#2273,.T.);
#998=FACE_BOUND('',#2275,.T.);
#999=FACE_BOUND('',#2279,.T.);
#1000=FACE_BOUND('',#2281,.T.);
#1001=FACE_BOUND('',#2285,.T.);
#1002=FACE_BOUND('',#2287,.T.);
#1003=FACE_BOUND('',#2291,.T.);
#1004=FACE_BOUND('',#2293,.T.);
#1005=FACE_BOUND('',#2299,.T.);
#1006=PLANE('',#7953);
#1007=PLANE('',#7954);
#1008=PLANE('',#7955);
#1009=PLANE('',#7956);
#1010=PLANE('',#7957);
#1011=PLANE('',#7958);
#1012=PLANE('',#7960);
#1013=PLANE('',#7961);
#1014=PLANE('',#7962);
#1015=PLANE('',#7963);
#1016=PLANE('',#7964);
#1017=PLANE('',#7965);
#1018=PLANE('',#7967);
#1019=PLANE('',#7968);
#1020=PLANE('',#7969);
#1021=PLANE('',#7970);
#1022=PLANE('',#7971);
#1023=PLANE('',#7972);
#1024=PLANE('',#7977);
#1025=PLANE('',#8014);
#1026=PLANE('',#8015);
#1027=PLANE('',#8016);
#1028=PLANE('',#8017);
#1029=PLANE('',#8018);
#1030=PLANE('',#8019);
#1031=PLANE('',#8020);
#1032=PLANE('',#8021);
#1033=PLANE('',#8022);
#1034=PLANE('',#8023);
#1035=PLANE('',#8028);
#1036=PLANE('',#8038);
#1037=PLANE('',#8041);
#1038=PLANE('',#8049);
#1039=PLANE('',#8050);
#1040=PLANE('',#8058);
#1041=PLANE('',#8059);
#1042=PLANE('',#8067);
#1043=PLANE('',#8068);
#1044=PLANE('',#8076);
#1045=PLANE('',#8077);
#1046=PLANE('',#8085);
#1047=PLANE('',#8086);
#1048=PLANE('',#8091);
#1049=PLANE('',#8101);
#1050=PLANE('',#8104);
#1051=PLANE('',#8112);
#1052=PLANE('',#8113);
#1053=PLANE('',#8121);
#1054=PLANE('',#8122);
#1055=PLANE('',#8130);
#1056=PLANE('',#8131);
#1057=PLANE('',#8139);
#1058=PLANE('',#8140);
#1059=PLANE('',#8148);
#1060=PLANE('',#8149);
#1061=PLANE('',#8157);
#1062=PLANE('',#8158);
#1063=PLANE('',#8159);
#1064=PLANE('',#8160);
#1065=PLANE('',#8161);
#1066=PLANE('',#8162);
#1067=PLANE('',#8163);
#1068=PLANE('',#8164);
#1069=PLANE('',#8165);
#1070=PLANE('',#8166);
#1071=PLANE('',#8167);
#1072=PLANE('',#8173);
#1073=PLANE('',#8174);
#1074=PLANE('',#8175);
#1075=PLANE('',#8180);
#1076=PLANE('',#8181);
#1077=PLANE('',#8182);
#1078=PLANE('',#8185);
#1079=PLANE('',#8186);
#1080=PLANE('',#8187);
#1081=PLANE('',#8188);
#1082=PLANE('',#8189);
#1083=PLANE('',#8190);
#1084=PLANE('',#8191);
#1085=PLANE('',#8192);
#1086=PLANE('',#8193);
#1087=PLANE('',#8195);
#1088=PLANE('',#8203);
#1089=PLANE('',#8243);
#1090=PLANE('',#8244);
#1091=PLANE('',#8246);
#1092=PLANE('',#8249);
#1093=PLANE('',#8257);
#1094=PLANE('',#8258);
#1095=PLANE('',#8278);
#1096=PLANE('',#8279);
#1097=PLANE('',#8299);
#1098=PLANE('',#8300);
#1099=PLANE('',#8308);
#1100=PLANE('',#8309);
#1101=PLANE('',#8329);
#1102=PLANE('',#8330);
#1103=PLANE('',#8350);
#1104=PLANE('',#8351);
#1105=PLANE('',#8356);
#1106=PLANE('',#8357);
#1107=PLANE('',#8358);
#1108=PLANE('',#8359);
#1109=PLANE('',#8360);
#1110=PLANE('',#8361);
#1111=PLANE('',#8397);
#1112=PLANE('',#8398);
#1113=PLANE('',#8400);
#1114=PLANE('',#8403);
#1115=PLANE('',#8411);
#1116=PLANE('',#8412);
#1117=PLANE('',#8432);
#1118=PLANE('',#8433);
#1119=PLANE('',#8453);
#1120=PLANE('',#8454);
#1121=PLANE('',#8462);
#1122=PLANE('',#8463);
#1123=PLANE('',#8483);
#1124=PLANE('',#8484);
#1125=PLANE('',#8504);
#1126=PLANE('',#8505);
#1127=PLANE('',#8521);
#1128=PLANE('',#8524);
#1129=PLANE('',#8536);
#1130=PLANE('',#8545);
#1131=PLANE('',#8578);
#1132=PLANE('',#8583);
#1133=PLANE('',#8588);
#1134=PLANE('',#8593);
#1135=PLANE('',#8598);
#1136=PLANE('',#8603);
#1137=PLANE('',#8612);
#1138=PLANE('',#8616);
#1139=PLANE('',#8617);
#1140=PLANE('',#8619);
#1141=PLANE('',#8624);
#1142=PLANE('',#8627);
#1143=PLANE('',#8632);
#1144=PLANE('',#8641);
#1145=PLANE('',#8642);
#1146=PLANE('',#8643);
#1147=PLANE('',#8644);
#1148=PLANE('',#8645);
#1149=PLANE('',#8646);
#1150=PLANE('',#8647);
#1151=PLANE('',#8648);
#1152=PLANE('',#8649);
#1153=PLANE('',#8651);
#1154=PLANE('',#8659);
#1155=PLANE('',#8757);
#1156=PLANE('',#8758);
#1157=PLANE('',#8759);
#1158=PLANE('',#8760);
#1159=PLANE('',#8761);
#1160=PLANE('',#8762);
#1161=PLANE('',#8763);
#1162=PLANE('',#8764);
#1163=PLANE('',#8765);
#1164=PLANE('',#8770);
#1165=PLANE('',#8780);
#1166=PLANE('',#8783);
#1167=PLANE('',#8791);
#1168=PLANE('',#8792);
#1169=PLANE('',#8800);
#1170=PLANE('',#8801);
#1171=PLANE('',#8809);
#1172=PLANE('',#8810);
#1173=PLANE('',#8818);
#1174=PLANE('',#8819);
#1175=PLANE('',#8827);
#1176=PLANE('',#8828);
#1177=PLANE('',#8833);
#1178=PLANE('',#8843);
#1179=PLANE('',#8846);
#1180=PLANE('',#8854);
#1181=PLANE('',#8855);
#1182=PLANE('',#8863);
#1183=PLANE('',#8864);
#1184=PLANE('',#8872);
#1185=PLANE('',#8873);
#1186=PLANE('',#8881);
#1187=PLANE('',#8882);
#1188=PLANE('',#8890);
#1189=PLANE('',#8891);
#1190=PLANE('',#8893);
#1191=PLANE('',#8901);
#1192=PLANE('',#8909);
#1193=PLANE('',#8910);
#1194=PLANE('',#8911);
#1195=PLANE('',#8912);
#1196=PLANE('',#8913);
#1197=PLANE('',#8914);
#1198=PLANE('',#8915);
#1199=PLANE('',#8916);
#1200=PLANE('',#8917);
#1201=FACE_OUTER_BOUND('',#1621,.T.);
#1202=FACE_OUTER_BOUND('',#1622,.T.);
#1203=FACE_OUTER_BOUND('',#1623,.T.);
#1204=FACE_OUTER_BOUND('',#1624,.T.);
#1205=FACE_OUTER_BOUND('',#1625,.T.);
#1206=FACE_OUTER_BOUND('',#1626,.T.);
#1207=FACE_OUTER_BOUND('',#1627,.T.);
#1208=FACE_OUTER_BOUND('',#1628,.T.);
#1209=FACE_OUTER_BOUND('',#1629,.T.);
#1210=FACE_OUTER_BOUND('',#1634,.T.);
#1211=FACE_OUTER_BOUND('',#1639,.T.);
#1212=FACE_OUTER_BOUND('',#1640,.T.);
#1213=FACE_OUTER_BOUND('',#1641,.T.);
#1214=FACE_OUTER_BOUND('',#1642,.T.);
#1215=FACE_OUTER_BOUND('',#1643,.T.);
#1216=FACE_OUTER_BOUND('',#1644,.T.);
#1217=FACE_OUTER_BOUND('',#1645,.T.);
#1218=FACE_OUTER_BOUND('',#1646,.T.);
#1219=FACE_OUTER_BOUND('',#1647,.T.);
#1220=FACE_OUTER_BOUND('',#1648,.T.);
#1221=FACE_OUTER_BOUND('',#1649,.T.);
#1222=FACE_OUTER_BOUND('',#1650,.T.);
#1223=FACE_OUTER_BOUND('',#1651,.T.);
#1224=FACE_OUTER_BOUND('',#1652,.T.);
#1225=FACE_OUTER_BOUND('',#1653,.T.);
#1226=FACE_OUTER_BOUND('',#1654,.T.);
#1227=FACE_OUTER_BOUND('',#1655,.T.);
#1228=FACE_OUTER_BOUND('',#1656,.T.);
#1229=FACE_OUTER_BOUND('',#1657,.T.);
#1230=FACE_OUTER_BOUND('',#1658,.T.);
#1231=FACE_OUTER_BOUND('',#1659,.T.);
#1232=FACE_OUTER_BOUND('',#1660,.T.);
#1233=FACE_OUTER_BOUND('',#1661,.T.);
#1234=FACE_OUTER_BOUND('',#1662,.T.);
#1235=FACE_OUTER_BOUND('',#1663,.T.);
#1236=FACE_OUTER_BOUND('',#1664,.T.);
#1237=FACE_OUTER_BOUND('',#1665,.T.);
#1238=FACE_OUTER_BOUND('',#1670,.T.);
#1239=FACE_OUTER_BOUND('',#1671,.T.);
#1240=FACE_OUTER_BOUND('',#1676,.T.);
#1241=FACE_OUTER_BOUND('',#1677,.T.);
#1242=FACE_OUTER_BOUND('',#1678,.T.);
#1243=FACE_OUTER_BOUND('',#1687,.T.);
#1244=FACE_OUTER_BOUND('',#1688,.T.);
#1245=FACE_OUTER_BOUND('',#1697,.T.);
#1246=FACE_OUTER_BOUND('',#1699,.T.);
#1247=FACE_OUTER_BOUND('',#1700,.T.);
#1248=FACE_OUTER_BOUND('',#1701,.T.);
#1249=FACE_OUTER_BOUND('',#1702,.T.);
#1250=FACE_OUTER_BOUND('',#1703,.T.);
#1251=FACE_OUTER_BOUND('',#1704,.T.);
#1252=FACE_OUTER_BOUND('',#1705,.T.);
#1253=FACE_OUTER_BOUND('',#1710,.T.);
#1254=FACE_OUTER_BOUND('',#1715,.T.);
#1255=FACE_OUTER_BOUND('',#1716,.T.);
#1256=FACE_OUTER_BOUND('',#1717,.T.);
#1257=FACE_OUTER_BOUND('',#1718,.T.);
#1258=FACE_OUTER_BOUND('',#1719,.T.);
#1259=FACE_OUTER_BOUND('',#1721,.T.);
#1260=FACE_OUTER_BOUND('',#1722,.T.);
#1261=FACE_OUTER_BOUND('',#1723,.T.);
#1262=FACE_OUTER_BOUND('',#1725,.T.);
#1263=FACE_OUTER_BOUND('',#1727,.T.);
#1264=FACE_OUTER_BOUND('',#1728,.T.);
#1265=FACE_OUTER_BOUND('',#1729,.T.);
#1266=FACE_OUTER_BOUND('',#1731,.T.);
#1267=FACE_OUTER_BOUND('',#1733,.T.);
#1268=FACE_OUTER_BOUND('',#1734,.T.);
#1269=FACE_OUTER_BOUND('',#1735,.T.);
#1270=FACE_OUTER_BOUND('',#1737,.T.);
#1271=FACE_OUTER_BOUND('',#1739,.T.);
#1272=FACE_OUTER_BOUND('',#1740,.T.);
#1273=FACE_OUTER_BOUND('',#1741,.T.);
#1274=FACE_OUTER_BOUND('',#1743,.T.);
#1275=FACE_OUTER_BOUND('',#1745,.T.);
#1276=FACE_OUTER_BOUND('',#1746,.T.);
#1277=FACE_OUTER_BOUND('',#1747,.T.);
#1278=FACE_OUTER_BOUND('',#1748,.T.);
#1279=FACE_OUTER_BOUND('',#1749,.T.);
#1280=FACE_OUTER_BOUND('',#1750,.T.);
#1281=FACE_OUTER_BOUND('',#1755,.T.);
#1282=FACE_OUTER_BOUND('',#1760,.T.);
#1283=FACE_OUTER_BOUND('',#1761,.T.);
#1284=FACE_OUTER_BOUND('',#1762,.T.);
#1285=FACE_OUTER_BOUND('',#1763,.T.);
#1286=FACE_OUTER_BOUND('',#1764,.T.);
#1287=FACE_OUTER_BOUND('',#1766,.T.);
#1288=FACE_OUTER_BOUND('',#1767,.T.);
#1289=FACE_OUTER_BOUND('',#1768,.T.);
#1290=FACE_OUTER_BOUND('',#1770,.T.);
#1291=FACE_OUTER_BOUND('',#1772,.T.);
#1292=FACE_OUTER_BOUND('',#1773,.T.);
#1293=FACE_OUTER_BOUND('',#1774,.T.);
#1294=FACE_OUTER_BOUND('',#1776,.T.);
#1295=FACE_OUTER_BOUND('',#1778,.T.);
#1296=FACE_OUTER_BOUND('',#1779,.T.);
#1297=FACE_OUTER_BOUND('',#1780,.T.);
#1298=FACE_OUTER_BOUND('',#1782,.T.);
#1299=FACE_OUTER_BOUND('',#1784,.T.);
#1300=FACE_OUTER_BOUND('',#1785,.T.);
#1301=FACE_OUTER_BOUND('',#1786,.T.);
#1302=FACE_OUTER_BOUND('',#1788,.T.);
#1303=FACE_OUTER_BOUND('',#1790,.T.);
#1304=FACE_OUTER_BOUND('',#1791,.T.);
#1305=FACE_OUTER_BOUND('',#1792,.T.);
#1306=FACE_OUTER_BOUND('',#1793,.T.);
#1307=FACE_OUTER_BOUND('',#1795,.T.);
#1308=FACE_OUTER_BOUND('',#1796,.T.);
#1309=FACE_OUTER_BOUND('',#1797,.T.);
#1310=FACE_OUTER_BOUND('',#1798,.T.);
#1311=FACE_OUTER_BOUND('',#1799,.T.);
#1312=FACE_OUTER_BOUND('',#1801,.T.);
#1313=FACE_OUTER_BOUND('',#1802,.T.);
#1314=FACE_OUTER_BOUND('',#1804,.T.);
#1315=FACE_OUTER_BOUND('',#1805,.T.);
#1316=FACE_OUTER_BOUND('',#1807,.T.);
#1317=FACE_OUTER_BOUND('',#1808,.T.);
#1318=FACE_OUTER_BOUND('',#1809,.T.);
#1319=FACE_OUTER_BOUND('',#1810,.T.);
#1320=FACE_OUTER_BOUND('',#1811,.T.);
#1321=FACE_OUTER_BOUND('',#1812,.T.);
#1322=FACE_OUTER_BOUND('',#1813,.T.);
#1323=FACE_OUTER_BOUND('',#1814,.T.);
#1324=FACE_OUTER_BOUND('',#1815,.T.);
#1325=FACE_OUTER_BOUND('',#1816,.T.);
#1326=FACE_OUTER_BOUND('',#1817,.T.);
#1327=FACE_OUTER_BOUND('',#1818,.T.);
#1328=FACE_OUTER_BOUND('',#1819,.T.);
#1329=FACE_OUTER_BOUND('',#1820,.T.);
#1330=FACE_OUTER_BOUND('',#1821,.T.);
#1331=FACE_OUTER_BOUND('',#1822,.T.);
#1332=FACE_OUTER_BOUND('',#1823,.T.);
#1333=FACE_OUTER_BOUND('',#1824,.T.);
#1334=FACE_OUTER_BOUND('',#1825,.T.);
#1335=FACE_OUTER_BOUND('',#1826,.T.);
#1336=FACE_OUTER_BOUND('',#1827,.T.);
#1337=FACE_OUTER_BOUND('',#1828,.T.);
#1338=FACE_OUTER_BOUND('',#1829,.T.);
#1339=FACE_OUTER_BOUND('',#1831,.T.);
#1340=FACE_OUTER_BOUND('',#1832,.T.);
#1341=FACE_OUTER_BOUND('',#1833,.T.);
#1342=FACE_OUTER_BOUND('',#1834,.T.);
#1343=FACE_OUTER_BOUND('',#1835,.T.);
#1344=FACE_OUTER_BOUND('',#1836,.T.);
#1345=FACE_OUTER_BOUND('',#1837,.T.);
#1346=FACE_OUTER_BOUND('',#1838,.T.);
#1347=FACE_OUTER_BOUND('',#1839,.T.);
#1348=FACE_OUTER_BOUND('',#1840,.T.);
#1349=FACE_OUTER_BOUND('',#1841,.T.);
#1350=FACE_OUTER_BOUND('',#1842,.T.);
#1351=FACE_OUTER_BOUND('',#1843,.T.);
#1352=FACE_OUTER_BOUND('',#1844,.T.);
#1353=FACE_OUTER_BOUND('',#1845,.T.);
#1354=FACE_OUTER_BOUND('',#1856,.T.);
#1355=FACE_OUTER_BOUND('',#1857,.T.);
#1356=FACE_OUTER_BOUND('',#1858,.T.);
#1357=FACE_OUTER_BOUND('',#1869,.T.);
#1358=FACE_OUTER_BOUND('',#1870,.T.);
#1359=FACE_OUTER_BOUND('',#1871,.T.);
#1360=FACE_OUTER_BOUND('',#1873,.T.);
#1361=FACE_OUTER_BOUND('',#1875,.T.);
#1362=FACE_OUTER_BOUND('',#1876,.T.);
#1363=FACE_OUTER_BOUND('',#1877,.T.);
#1364=FACE_OUTER_BOUND('',#1878,.T.);
#1365=FACE_OUTER_BOUND('',#1879,.T.);
#1366=FACE_OUTER_BOUND('',#1880,.T.);
#1367=FACE_OUTER_BOUND('',#1881,.T.);
#1368=FACE_OUTER_BOUND('',#1887,.T.);
#1369=FACE_OUTER_BOUND('',#1893,.T.);
#1370=FACE_OUTER_BOUND('',#1894,.T.);
#1371=FACE_OUTER_BOUND('',#1895,.T.);
#1372=FACE_OUTER_BOUND('',#1896,.T.);
#1373=FACE_OUTER_BOUND('',#1897,.T.);
#1374=FACE_OUTER_BOUND('',#1898,.T.);
#1375=FACE_OUTER_BOUND('',#1899,.T.);
#1376=FACE_OUTER_BOUND('',#1905,.T.);
#1377=FACE_OUTER_BOUND('',#1911,.T.);
#1378=FACE_OUTER_BOUND('',#1912,.T.);
#1379=FACE_OUTER_BOUND('',#1913,.T.);
#1380=FACE_OUTER_BOUND('',#1915,.T.);
#1381=FACE_OUTER_BOUND('',#1917,.T.);
#1382=FACE_OUTER_BOUND('',#1918,.T.);
#1383=FACE_OUTER_BOUND('',#1919,.T.);
#1384=FACE_OUTER_BOUND('',#1920,.T.);
#1385=FACE_OUTER_BOUND('',#1921,.T.);
#1386=FACE_OUTER_BOUND('',#1922,.T.);
#1387=FACE_OUTER_BOUND('',#1923,.T.);
#1388=FACE_OUTER_BOUND('',#1929,.T.);
#1389=FACE_OUTER_BOUND('',#1935,.T.);
#1390=FACE_OUTER_BOUND('',#1936,.T.);
#1391=FACE_OUTER_BOUND('',#1937,.T.);
#1392=FACE_OUTER_BOUND('',#1938,.T.);
#1393=FACE_OUTER_BOUND('',#1939,.T.);
#1394=FACE_OUTER_BOUND('',#1940,.T.);
#1395=FACE_OUTER_BOUND('',#1941,.T.);
#1396=FACE_OUTER_BOUND('',#1947,.T.);
#1397=FACE_OUTER_BOUND('',#1953,.T.);
#1398=FACE_OUTER_BOUND('',#1954,.T.);
#1399=FACE_OUTER_BOUND('',#1955,.T.);
#1400=FACE_OUTER_BOUND('',#1957,.T.);
#1401=FACE_OUTER_BOUND('',#1958,.T.);
#1402=FACE_OUTER_BOUND('',#1960,.T.);
#1403=FACE_OUTER_BOUND('',#1961,.T.);
#1404=FACE_OUTER_BOUND('',#1962,.T.);
#1405=FACE_OUTER_BOUND('',#1963,.T.);
#1406=FACE_OUTER_BOUND('',#1964,.T.);
#1407=FACE_OUTER_BOUND('',#1965,.T.);
#1408=FACE_OUTER_BOUND('',#1966,.T.);
#1409=FACE_OUTER_BOUND('',#1967,.T.);
#1410=FACE_OUTER_BOUND('',#1968,.T.);
#1411=FACE_OUTER_BOUND('',#1969,.T.);
#1412=FACE_OUTER_BOUND('',#1970,.T.);
#1413=FACE_OUTER_BOUND('',#1971,.T.);
#1414=FACE_OUTER_BOUND('',#1972,.T.);
#1415=FACE_OUTER_BOUND('',#1973,.T.);
#1416=FACE_OUTER_BOUND('',#1974,.T.);
#1417=FACE_OUTER_BOUND('',#1985,.T.);
#1418=FACE_OUTER_BOUND('',#1986,.T.);
#1419=FACE_OUTER_BOUND('',#1987,.T.);
#1420=FACE_OUTER_BOUND('',#1998,.T.);
#1421=FACE_OUTER_BOUND('',#1999,.T.);
#1422=FACE_OUTER_BOUND('',#2000,.T.);
#1423=FACE_OUTER_BOUND('',#2002,.T.);
#1424=FACE_OUTER_BOUND('',#2004,.T.);
#1425=FACE_OUTER_BOUND('',#2005,.T.);
#1426=FACE_OUTER_BOUND('',#2006,.T.);
#1427=FACE_OUTER_BOUND('',#2007,.T.);
#1428=FACE_OUTER_BOUND('',#2008,.T.);
#1429=FACE_OUTER_BOUND('',#2009,.T.);
#1430=FACE_OUTER_BOUND('',#2010,.T.);
#1431=FACE_OUTER_BOUND('',#2016,.T.);
#1432=FACE_OUTER_BOUND('',#2022,.T.);
#1433=FACE_OUTER_BOUND('',#2023,.T.);
#1434=FACE_OUTER_BOUND('',#2024,.T.);
#1435=FACE_OUTER_BOUND('',#2025,.T.);
#1436=FACE_OUTER_BOUND('',#2026,.T.);
#1437=FACE_OUTER_BOUND('',#2027,.T.);
#1438=FACE_OUTER_BOUND('',#2028,.T.);
#1439=FACE_OUTER_BOUND('',#2034,.T.);
#1440=FACE_OUTER_BOUND('',#2040,.T.);
#1441=FACE_OUTER_BOUND('',#2041,.T.);
#1442=FACE_OUTER_BOUND('',#2042,.T.);
#1443=FACE_OUTER_BOUND('',#2044,.T.);
#1444=FACE_OUTER_BOUND('',#2046,.T.);
#1445=FACE_OUTER_BOUND('',#2047,.T.);
#1446=FACE_OUTER_BOUND('',#2048,.T.);
#1447=FACE_OUTER_BOUND('',#2049,.T.);
#1448=FACE_OUTER_BOUND('',#2050,.T.);
#1449=FACE_OUTER_BOUND('',#2051,.T.);
#1450=FACE_OUTER_BOUND('',#2052,.T.);
#1451=FACE_OUTER_BOUND('',#2058,.T.);
#1452=FACE_OUTER_BOUND('',#2064,.T.);
#1453=FACE_OUTER_BOUND('',#2065,.T.);
#1454=FACE_OUTER_BOUND('',#2066,.T.);
#1455=FACE_OUTER_BOUND('',#2067,.T.);
#1456=FACE_OUTER_BOUND('',#2068,.T.);
#1457=FACE_OUTER_BOUND('',#2069,.T.);
#1458=FACE_OUTER_BOUND('',#2070,.T.);
#1459=FACE_OUTER_BOUND('',#2076,.T.);
#1460=FACE_OUTER_BOUND('',#2082,.T.);
#1461=FACE_OUTER_BOUND('',#2083,.T.);
#1462=FACE_OUTER_BOUND('',#2084,.T.);
#1463=FACE_OUTER_BOUND('',#2085,.T.);
#1464=FACE_OUTER_BOUND('',#2086,.T.);
#1465=FACE_OUTER_BOUND('',#2088,.T.);
#1466=FACE_OUTER_BOUND('',#2089,.T.);
#1467=FACE_OUTER_BOUND('',#2091,.T.);
#1468=FACE_OUTER_BOUND('',#2092,.T.);
#1469=FACE_OUTER_BOUND('',#2093,.T.);
#1470=FACE_OUTER_BOUND('',#2094,.T.);
#1471=FACE_OUTER_BOUND('',#2096,.T.);
#1472=FACE_OUTER_BOUND('',#2097,.T.);
#1473=FACE_OUTER_BOUND('',#2098,.T.);
#1474=FACE_OUTER_BOUND('',#2099,.T.);
#1475=FACE_OUTER_BOUND('',#2101,.T.);
#1476=FACE_OUTER_BOUND('',#2102,.T.);
#1477=FACE_OUTER_BOUND('',#2103,.T.);
#1478=FACE_OUTER_BOUND('',#2104,.T.);
#1479=FACE_OUTER_BOUND('',#2105,.T.);
#1480=FACE_OUTER_BOUND('',#2106,.T.);
#1481=FACE_OUTER_BOUND('',#2107,.T.);
#1482=FACE_OUTER_BOUND('',#2108,.T.);
#1483=FACE_OUTER_BOUND('',#2109,.T.);
#1484=FACE_OUTER_BOUND('',#2110,.T.);
#1485=FACE_OUTER_BOUND('',#2111,.T.);
#1486=FACE_OUTER_BOUND('',#2112,.T.);
#1487=FACE_OUTER_BOUND('',#2113,.T.);
#1488=FACE_OUTER_BOUND('',#2114,.T.);
#1489=FACE_OUTER_BOUND('',#2115,.T.);
#1490=FACE_OUTER_BOUND('',#2116,.T.);
#1491=FACE_OUTER_BOUND('',#2117,.T.);
#1492=FACE_OUTER_BOUND('',#2118,.T.);
#1493=FACE_OUTER_BOUND('',#2119,.T.);
#1494=FACE_OUTER_BOUND('',#2120,.T.);
#1495=FACE_OUTER_BOUND('',#2121,.T.);
#1496=FACE_OUTER_BOUND('',#2122,.T.);
#1497=FACE_OUTER_BOUND('',#2123,.T.);
#1498=FACE_OUTER_BOUND('',#2124,.T.);
#1499=FACE_OUTER_BOUND('',#2125,.T.);
#1500=FACE_OUTER_BOUND('',#2126,.T.);
#1501=FACE_OUTER_BOUND('',#2127,.T.);
#1502=FACE_OUTER_BOUND('',#2129,.T.);
#1503=FACE_OUTER_BOUND('',#2130,.T.);
#1504=FACE_OUTER_BOUND('',#2132,.T.);
#1505=FACE_OUTER_BOUND('',#2133,.T.);
#1506=FACE_OUTER_BOUND('',#2135,.T.);
#1507=FACE_OUTER_BOUND('',#2136,.T.);
#1508=FACE_OUTER_BOUND('',#2138,.T.);
#1509=FACE_OUTER_BOUND('',#2139,.T.);
#1510=FACE_OUTER_BOUND('',#2141,.T.);
#1511=FACE_OUTER_BOUND('',#2142,.T.);
#1512=FACE_OUTER_BOUND('',#2143,.T.);
#1513=FACE_OUTER_BOUND('',#2144,.T.);
#1514=FACE_OUTER_BOUND('',#2145,.T.);
#1515=FACE_OUTER_BOUND('',#2146,.T.);
#1516=FACE_OUTER_BOUND('',#2147,.T.);
#1517=FACE_OUTER_BOUND('',#2148,.T.);
#1518=FACE_OUTER_BOUND('',#2149,.T.);
#1519=FACE_OUTER_BOUND('',#2150,.T.);
#1520=FACE_OUTER_BOUND('',#2151,.T.);
#1521=FACE_OUTER_BOUND('',#2152,.T.);
#1522=FACE_OUTER_BOUND('',#2153,.T.);
#1523=FACE_OUTER_BOUND('',#2154,.T.);
#1524=FACE_OUTER_BOUND('',#2155,.T.);
#1525=FACE_OUTER_BOUND('',#2157,.T.);
#1526=FACE_OUTER_BOUND('',#2158,.T.);
#1527=FACE_OUTER_BOUND('',#2159,.T.);
#1528=FACE_OUTER_BOUND('',#2160,.T.);
#1529=FACE_OUTER_BOUND('',#2161,.T.);
#1530=FACE_OUTER_BOUND('',#2162,.T.);
#1531=FACE_OUTER_BOUND('',#2163,.T.);
#1532=FACE_OUTER_BOUND('',#2164,.T.);
#1533=FACE_OUTER_BOUND('',#2165,.T.);
#1534=FACE_OUTER_BOUND('',#2166,.T.);
#1535=FACE_OUTER_BOUND('',#2167,.T.);
#1536=FACE_OUTER_BOUND('',#2168,.T.);
#1537=FACE_OUTER_BOUND('',#2169,.T.);
#1538=FACE_OUTER_BOUND('',#2170,.T.);
#1539=FACE_OUTER_BOUND('',#2171,.T.);
#1540=FACE_OUTER_BOUND('',#2172,.T.);
#1541=FACE_OUTER_BOUND('',#2173,.T.);
#1542=FACE_OUTER_BOUND('',#2178,.T.);
#1543=FACE_OUTER_BOUND('',#2183,.T.);
#1544=FACE_OUTER_BOUND('',#2192,.T.);
#1545=FACE_OUTER_BOUND('',#2193,.T.);
#1546=FACE_OUTER_BOUND('',#2202,.T.);
#1547=FACE_OUTER_BOUND('',#2203,.T.);
#1548=FACE_OUTER_BOUND('',#2204,.T.);
#1549=FACE_OUTER_BOUND('',#2205,.T.);
#1550=FACE_OUTER_BOUND('',#2206,.T.);
#1551=FACE_OUTER_BOUND('',#2207,.T.);
#1552=FACE_OUTER_BOUND('',#2208,.T.);
#1553=FACE_OUTER_BOUND('',#2209,.T.);
#1554=FACE_OUTER_BOUND('',#2214,.T.);
#1555=FACE_OUTER_BOUND('',#2219,.T.);
#1556=FACE_OUTER_BOUND('',#2220,.T.);
#1557=FACE_OUTER_BOUND('',#2221,.T.);
#1558=FACE_OUTER_BOUND('',#2222,.T.);
#1559=FACE_OUTER_BOUND('',#2223,.T.);
#1560=FACE_OUTER_BOUND('',#2225,.T.);
#1561=FACE_OUTER_BOUND('',#2226,.T.);
#1562=FACE_OUTER_BOUND('',#2227,.T.);
#1563=FACE_OUTER_BOUND('',#2229,.T.);
#1564=FACE_OUTER_BOUND('',#2231,.T.);
#1565=FACE_OUTER_BOUND('',#2232,.T.);
#1566=FACE_OUTER_BOUND('',#2233,.T.);
#1567=FACE_OUTER_BOUND('',#2235,.T.);
#1568=FACE_OUTER_BOUND('',#2237,.T.);
#1569=FACE_OUTER_BOUND('',#2238,.T.);
#1570=FACE_OUTER_BOUND('',#2239,.T.);
#1571=FACE_OUTER_BOUND('',#2241,.T.);
#1572=FACE_OUTER_BOUND('',#2243,.T.);
#1573=FACE_OUTER_BOUND('',#2244,.T.);
#1574=FACE_OUTER_BOUND('',#2245,.T.);
#1575=FACE_OUTER_BOUND('',#2247,.T.);
#1576=FACE_OUTER_BOUND('',#2249,.T.);
#1577=FACE_OUTER_BOUND('',#2250,.T.);
#1578=FACE_OUTER_BOUND('',#2251,.T.);
#1579=FACE_OUTER_BOUND('',#2252,.T.);
#1580=FACE_OUTER_BOUND('',#2253,.T.);
#1581=FACE_OUTER_BOUND('',#2254,.T.);
#1582=FACE_OUTER_BOUND('',#2259,.T.);
#1583=FACE_OUTER_BOUND('',#2264,.T.);
#1584=FACE_OUTER_BOUND('',#2265,.T.);
#1585=FACE_OUTER_BOUND('',#2266,.T.);
#1586=FACE_OUTER_BOUND('',#2267,.T.);
#1587=FACE_OUTER_BOUND('',#2268,.T.);
#1588=FACE_OUTER_BOUND('',#2270,.T.);
#1589=FACE_OUTER_BOUND('',#2271,.T.);
#1590=FACE_OUTER_BOUND('',#2272,.T.);
#1591=FACE_OUTER_BOUND('',#2274,.T.);
#1592=FACE_OUTER_BOUND('',#2276,.T.);
#1593=FACE_OUTER_BOUND('',#2277,.T.);
#1594=FACE_OUTER_BOUND('',#2278,.T.);
#1595=FACE_OUTER_BOUND('',#2280,.T.);
#1596=FACE_OUTER_BOUND('',#2282,.T.);
#1597=FACE_OUTER_BOUND('',#2283,.T.);
#1598=FACE_OUTER_BOUND('',#2284,.T.);
#1599=FACE_OUTER_BOUND('',#2286,.T.);
#1600=FACE_OUTER_BOUND('',#2288,.T.);
#1601=FACE_OUTER_BOUND('',#2289,.T.);
#1602=FACE_OUTER_BOUND('',#2290,.T.);
#1603=FACE_OUTER_BOUND('',#2292,.T.);
#1604=FACE_OUTER_BOUND('',#2294,.T.);
#1605=FACE_OUTER_BOUND('',#2295,.T.);
#1606=FACE_OUTER_BOUND('',#2296,.T.);
#1607=FACE_OUTER_BOUND('',#2297,.T.);
#1608=FACE_OUTER_BOUND('',#2298,.T.);
#1609=FACE_OUTER_BOUND('',#2300,.T.);
#1610=FACE_OUTER_BOUND('',#2301,.T.);
#1611=FACE_OUTER_BOUND('',#2302,.T.);
#1612=FACE_OUTER_BOUND('',#2303,.T.);
#1613=FACE_OUTER_BOUND('',#2304,.T.);
#1614=FACE_OUTER_BOUND('',#2305,.T.);
#1615=FACE_OUTER_BOUND('',#2306,.T.);
#1616=FACE_OUTER_BOUND('',#2307,.T.);
#1617=FACE_OUTER_BOUND('',#2308,.T.);
#1618=FACE_OUTER_BOUND('',#2309,.T.);
#1619=FACE_OUTER_BOUND('',#2310,.T.);
#1620=FACE_OUTER_BOUND('',#2311,.T.);
#1621=EDGE_LOOP('',(#4988,#4989,#4990,#4991));
#1622=EDGE_LOOP('',(#4992,#4993,#4994,#4995));
#1623=EDGE_LOOP('',(#4996,#4997,#4998,#4999));
#1624=EDGE_LOOP('',(#5000,#5001,#5002,#5003));
#1625=EDGE_LOOP('',(#5004,#5005,#5006,#5007));
#1626=EDGE_LOOP('',(#5008,#5009,#5010,#5011));
#1627=EDGE_LOOP('',(#5012,#5013,#5014,#5015));
#1628=EDGE_LOOP('',(#5016,#5017,#5018,#5019));
#1629=EDGE_LOOP('',(#5020,#5021,#5022,#5023));
#1630=EDGE_LOOP('',(#5024));
#1631=EDGE_LOOP('',(#5025));
#1632=EDGE_LOOP('',(#5026));
#1633=EDGE_LOOP('',(#5027));
#1634=EDGE_LOOP('',(#5028,#5029,#5030,#5031));
#1635=EDGE_LOOP('',(#5032));
#1636=EDGE_LOOP('',(#5033));
#1637=EDGE_LOOP('',(#5034));
#1638=EDGE_LOOP('',(#5035));
#1639=EDGE_LOOP('',(#5036,#5037,#5038,#5039));
#1640=EDGE_LOOP('',(#5040,#5041,#5042,#5043));
#1641=EDGE_LOOP('',(#5044,#5045,#5046,#5047));
#1642=EDGE_LOOP('',(#5048,#5049,#5050,#5051));
#1643=EDGE_LOOP('',(#5052,#5053,#5054,#5055));
#1644=EDGE_LOOP('',(#5056,#5057,#5058,#5059));
#1645=EDGE_LOOP('',(#5060,#5061,#5062,#5063));
#1646=EDGE_LOOP('',(#5064,#5065,#5066,#5067));
#1647=EDGE_LOOP('',(#5068,#5069,#5070,#5071));
#1648=EDGE_LOOP('',(#5072,#5073,#5074,#5075));
#1649=EDGE_LOOP('',(#5076,#5077,#5078,#5079));
#1650=EDGE_LOOP('',(#5080,#5081,#5082,#5083));
#1651=EDGE_LOOP('',(#5084,#5085,#5086,#5087));
#1652=EDGE_LOOP('',(#5088));
#1653=EDGE_LOOP('',(#5089,#5090,#5091,#5092));
#1654=EDGE_LOOP('',(#5093,#5094,#5095,#5096));
#1655=EDGE_LOOP('',(#5097,#5098,#5099,#5100));
#1656=EDGE_LOOP('',(#5101,#5102,#5103,#5104));
#1657=EDGE_LOOP('',(#5105,#5106,#5107,#5108));
#1658=EDGE_LOOP('',(#5109,#5110,#5111,#5112));
#1659=EDGE_LOOP('',(#5113,#5114,#5115,#5116));
#1660=EDGE_LOOP('',(#5117,#5118,#5119,#5120));
#1661=EDGE_LOOP('',(#5121,#5122,#5123,#5124));
#1662=EDGE_LOOP('',(#5125,#5126,#5127,#5128));
#1663=EDGE_LOOP('',(#5129,#5130,#5131,#5132));
#1664=EDGE_LOOP('',(#5133,#5134,#5135,#5136));
#1665=EDGE_LOOP('',(#5137,#5138,#5139,#5140,#5141,#5142,#5143,#5144));
#1666=EDGE_LOOP('',(#5145));
#1667=EDGE_LOOP('',(#5146));
#1668=EDGE_LOOP('',(#5147));
#1669=EDGE_LOOP('',(#5148));
#1670=EDGE_LOOP('',(#5149,#5150,#5151,#5152));
#1671=EDGE_LOOP('',(#5153,#5154,#5155,#5156));
#1672=EDGE_LOOP('',(#5157));
#1673=EDGE_LOOP('',(#5158));
#1674=EDGE_LOOP('',(#5159));
#1675=EDGE_LOOP('',(#5160));
#1676=EDGE_LOOP('',(#5161,#5162,#5163,#5164));
#1677=EDGE_LOOP('',(#5165,#5166,#5167,#5168));
#1678=EDGE_LOOP('',(#5169,#5170,#5171,#5172));
#1679=EDGE_LOOP('',(#5173));
#1680=EDGE_LOOP('',(#5174));
#1681=EDGE_LOOP('',(#5175));
#1682=EDGE_LOOP('',(#5176));
#1683=EDGE_LOOP('',(#5177));
#1684=EDGE_LOOP('',(#5178));
#1685=EDGE_LOOP('',(#5179));
#1686=EDGE_LOOP('',(#5180));
#1687=EDGE_LOOP('',(#5181,#5182,#5183,#5184));
#1688=EDGE_LOOP('',(#5185,#5186,#5187,#5188,#5189,#5190,#5191,#5192));
#1689=EDGE_LOOP('',(#5193));
#1690=EDGE_LOOP('',(#5194));
#1691=EDGE_LOOP('',(#5195));
#1692=EDGE_LOOP('',(#5196));
#1693=EDGE_LOOP('',(#5197));
#1694=EDGE_LOOP('',(#5198));
#1695=EDGE_LOOP('',(#5199));
#1696=EDGE_LOOP('',(#5200));
#1697=EDGE_LOOP('',(#5201,#5202,#5203,#5204));
#1698=EDGE_LOOP('',(#5205));
#1699=EDGE_LOOP('',(#5206,#5207,#5208,#5209));
#1700=EDGE_LOOP('',(#5210,#5211,#5212,#5213));
#1701=EDGE_LOOP('',(#5214));
#1702=EDGE_LOOP('',(#5215,#5216,#5217,#5218));
#1703=EDGE_LOOP('',(#5219,#5220,#5221,#5222));
#1704=EDGE_LOOP('',(#5223,#5224,#5225,#5226));
#1705=EDGE_LOOP('',(#5227));
#1706=EDGE_LOOP('',(#5228));
#1707=EDGE_LOOP('',(#5229));
#1708=EDGE_LOOP('',(#5230));
#1709=EDGE_LOOP('',(#5231));
#1710=EDGE_LOOP('',(#5232));
#1711=EDGE_LOOP('',(#5233));
#1712=EDGE_LOOP('',(#5234));
#1713=EDGE_LOOP('',(#5235));
#1714=EDGE_LOOP('',(#5236));
#1715=EDGE_LOOP('',(#5237,#5238,#5239,#5240));
#1716=EDGE_LOOP('',(#5241,#5242,#5243,#5244));
#1717=EDGE_LOOP('',(#5245,#5246,#5247,#5248));
#1718=EDGE_LOOP('',(#5249));
#1719=EDGE_LOOP('',(#5250));
#1720=EDGE_LOOP('',(#5251));
#1721=EDGE_LOOP('',(#5252,#5253,#5254,#5255));
#1722=EDGE_LOOP('',(#5256,#5257,#5258,#5259));
#1723=EDGE_LOOP('',(#5260));
#1724=EDGE_LOOP('',(#5261));
#1725=EDGE_LOOP('',(#5262));
#1726=EDGE_LOOP('',(#5263));
#1727=EDGE_LOOP('',(#5264,#5265,#5266,#5267));
#1728=EDGE_LOOP('',(#5268,#5269,#5270,#5271));
#1729=EDGE_LOOP('',(#5272));
#1730=EDGE_LOOP('',(#5273));
#1731=EDGE_LOOP('',(#5274));
#1732=EDGE_LOOP('',(#5275));
#1733=EDGE_LOOP('',(#5276,#5277,#5278,#5279));
#1734=EDGE_LOOP('',(#5280,#5281,#5282,#5283));
#1735=EDGE_LOOP('',(#5284));
#1736=EDGE_LOOP('',(#5285));
#1737=EDGE_LOOP('',(#5286));
#1738=EDGE_LOOP('',(#5287));
#1739=EDGE_LOOP('',(#5288,#5289,#5290,#5291));
#1740=EDGE_LOOP('',(#5292,#5293,#5294,#5295));
#1741=EDGE_LOOP('',(#5296));
#1742=EDGE_LOOP('',(#5297));
#1743=EDGE_LOOP('',(#5298));
#1744=EDGE_LOOP('',(#5299));
#1745=EDGE_LOOP('',(#5300,#5301,#5302,#5303));
#1746=EDGE_LOOP('',(#5304));
#1747=EDGE_LOOP('',(#5305,#5306,#5307,#5308));
#1748=EDGE_LOOP('',(#5309,#5310,#5311,#5312));
#1749=EDGE_LOOP('',(#5313,#5314,#5315,#5316));
#1750=EDGE_LOOP('',(#5317));
#1751=EDGE_LOOP('',(#5318));
#1752=EDGE_LOOP('',(#5319));
#1753=EDGE_LOOP('',(#5320));
#1754=EDGE_LOOP('',(#5321));
#1755=EDGE_LOOP('',(#5322));
#1756=EDGE_LOOP('',(#5323));
#1757=EDGE_LOOP('',(#5324));
#1758=EDGE_LOOP('',(#5325));
#1759=EDGE_LOOP('',(#5326));
#1760=EDGE_LOOP('',(#5327,#5328,#5329,#5330));
#1761=EDGE_LOOP('',(#5331,#5332,#5333,#5334));
#1762=EDGE_LOOP('',(#5335,#5336,#5337,#5338));
#1763=EDGE_LOOP('',(#5339));
#1764=EDGE_LOOP('',(#5340));
#1765=EDGE_LOOP('',(#5341));
#1766=EDGE_LOOP('',(#5342,#5343,#5344,#5345));
#1767=EDGE_LOOP('',(#5346,#5347,#5348,#5349));
#1768=EDGE_LOOP('',(#5350));
#1769=EDGE_LOOP('',(#5351));
#1770=EDGE_LOOP('',(#5352));
#1771=EDGE_LOOP('',(#5353));
#1772=EDGE_LOOP('',(#5354,#5355,#5356,#5357));
#1773=EDGE_LOOP('',(#5358,#5359,#5360,#5361));
#1774=EDGE_LOOP('',(#5362));
#1775=EDGE_LOOP('',(#5363));
#1776=EDGE_LOOP('',(#5364));
#1777=EDGE_LOOP('',(#5365));
#1778=EDGE_LOOP('',(#5366,#5367,#5368,#5369));
#1779=EDGE_LOOP('',(#5370,#5371,#5372,#5373));
#1780=EDGE_LOOP('',(#5374));
#1781=EDGE_LOOP('',(#5375));
#1782=EDGE_LOOP('',(#5376));
#1783=EDGE_LOOP('',(#5377));
#1784=EDGE_LOOP('',(#5378,#5379,#5380,#5381));
#1785=EDGE_LOOP('',(#5382,#5383,#5384,#5385));
#1786=EDGE_LOOP('',(#5386));
#1787=EDGE_LOOP('',(#5387));
#1788=EDGE_LOOP('',(#5388));
#1789=EDGE_LOOP('',(#5389));
#1790=EDGE_LOOP('',(#5390,#5391,#5392,#5393));
#1791=EDGE_LOOP('',(#5394,#5395,#5396,#5397));
#1792=EDGE_LOOP('',(#5398,#5399,#5400,#5401));
#1793=EDGE_LOOP('',(#5402,#5403,#5404,#5405));
#1794=EDGE_LOOP('',(#5406));
#1795=EDGE_LOOP('',(#5407,#5408,#5409,#5410,#5411,#5412,#5413,#5414));
#1796=EDGE_LOOP('',(#5415,#5416,#5417,#5418));
#1797=EDGE_LOOP('',(#5419,#5420,#5421,#5422,#5423,#5424));
#1798=EDGE_LOOP('',(#5425,#5426,#5427,#5428));
#1799=EDGE_LOOP('',(#5429,#5430,#5431,#5432));
#1800=EDGE_LOOP('',(#5433));
#1801=EDGE_LOOP('',(#5434,#5435,#5436,#5437));
#1802=EDGE_LOOP('',(#5438,#5439,#5440,#5441,#5442,#5443));
#1803=EDGE_LOOP('',(#5444));
#1804=EDGE_LOOP('',(#5445,#5446,#5447,#5448));
#1805=EDGE_LOOP('',(#5449,#5450,#5451,#5452,#5453,#5454));
#1806=EDGE_LOOP('',(#5455));
#1807=EDGE_LOOP('',(#5456,#5457,#5458,#5459,#5460,#5461,#5462));
#1808=EDGE_LOOP('',(#5463));
#1809=EDGE_LOOP('',(#5464,#5465,#5466));
#1810=EDGE_LOOP('',(#5467,#5468));
#1811=EDGE_LOOP('',(#5469,#5470,#5471,#5472,#5473,#5474,#5475));
#1812=EDGE_LOOP('',(#5476));
#1813=EDGE_LOOP('',(#5477,#5478));
#1814=EDGE_LOOP('',(#5479,#5480));
#1815=EDGE_LOOP('',(#5481,#5482,#5483,#5484,#5485,#5486,#5487,#5488,#5489));
#1816=EDGE_LOOP('',(#5490,#5491,#5492,#5493));
#1817=EDGE_LOOP('',(#5494,#5495,#5496,#5497));
#1818=EDGE_LOOP('',(#5498,#5499,#5500,#5501));
#1819=EDGE_LOOP('',(#5502,#5503,#5504,#5505));
#1820=EDGE_LOOP('',(#5506,#5507,#5508,#5509));
#1821=EDGE_LOOP('',(#5510,#5511,#5512,#5513));
#1822=EDGE_LOOP('',(#5514,#5515,#5516,#5517,#5518,#5519));
#1823=EDGE_LOOP('',(#5520,#5521,#5522,#5523,#5524,#5525));
#1824=EDGE_LOOP('',(#5526));
#1825=EDGE_LOOP('',(#5527));
#1826=EDGE_LOOP('',(#5528,#5529,#5530,#5531));
#1827=EDGE_LOOP('',(#5532,#5533,#5534,#5535));
#1828=EDGE_LOOP('',(#5536,#5537,#5538,#5539));
#1829=EDGE_LOOP('',(#5540));
#1830=EDGE_LOOP('',(#5541));
#1831=EDGE_LOOP('',(#5542,#5543,#5544,#5545));
#1832=EDGE_LOOP('',(#5546,#5547,#5548,#5549));
#1833=EDGE_LOOP('',(#5550,#5551,#5552,#5553));
#1834=EDGE_LOOP('',(#5554,#5555,#5556,#5557));
#1835=EDGE_LOOP('',(#5558,#5559,#5560,#5561));
#1836=EDGE_LOOP('',(#5562,#5563,#5564,#5565));
#1837=EDGE_LOOP('',(#5566,#5567,#5568,#5569));
#1838=EDGE_LOOP('',(#5570,#5571,#5572,#5573));
#1839=EDGE_LOOP('',(#5574,#5575,#5576,#5577));
#1840=EDGE_LOOP('',(#5578,#5579,#5580,#5581));
#1841=EDGE_LOOP('',(#5582,#5583,#5584,#5585));
#1842=EDGE_LOOP('',(#5586,#5587,#5588,#5589));
#1843=EDGE_LOOP('',(#5590,#5591,#5592,#5593));
#1844=EDGE_LOOP('',(#5594,#5595,#5596,#5597));
#1845=EDGE_LOOP('',(#5598,#5599,#5600,#5601));
#1846=EDGE_LOOP('',(#5602));
#1847=EDGE_LOOP('',(#5603));
#1848=EDGE_LOOP('',(#5604));
#1849=EDGE_LOOP('',(#5605));
#1850=EDGE_LOOP('',(#5606));
#1851=EDGE_LOOP('',(#5607));
#1852=EDGE_LOOP('',(#5608));
#1853=EDGE_LOOP('',(#5609));
#1854=EDGE_LOOP('',(#5610));
#1855=EDGE_LOOP('',(#5611));
#1856=EDGE_LOOP('',(#5612,#5613,#5614,#5615));
#1857=EDGE_LOOP('',(#5616,#5617,#5618,#5619));
#1858=EDGE_LOOP('',(#5620,#5621,#5622,#5623));
#1859=EDGE_LOOP('',(#5624));
#1860=EDGE_LOOP('',(#5625));
#1861=EDGE_LOOP('',(#5626));
#1862=EDGE_LOOP('',(#5627));
#1863=EDGE_LOOP('',(#5628));
#1864=EDGE_LOOP('',(#5629));
#1865=EDGE_LOOP('',(#5630));
#1866=EDGE_LOOP('',(#5631));
#1867=EDGE_LOOP('',(#5632));
#1868=EDGE_LOOP('',(#5633));
#1869=EDGE_LOOP('',(#5634,#5635,#5636,#5637));
#1870=EDGE_LOOP('',(#5638,#5639,#5640,#5641));
#1871=EDGE_LOOP('',(#5642));
#1872=EDGE_LOOP('',(#5643));
#1873=EDGE_LOOP('',(#5644));
#1874=EDGE_LOOP('',(#5645));
#1875=EDGE_LOOP('',(#5646,#5647,#5648,#5649));
#1876=EDGE_LOOP('',(#5650,#5651,#5652,#5653));
#1877=EDGE_LOOP('',(#5654,#5655,#5656,#5657));
#1878=EDGE_LOOP('',(#5658,#5659,#5660,#5661));
#1879=EDGE_LOOP('',(#5662,#5663,#5664,#5665));
#1880=EDGE_LOOP('',(#5666,#5667,#5668,#5669));
#1881=EDGE_LOOP('',(#5670));
#1882=EDGE_LOOP('',(#5671));
#1883=EDGE_LOOP('',(#5672));
#1884=EDGE_LOOP('',(#5673));
#1885=EDGE_LOOP('',(#5674));
#1886=EDGE_LOOP('',(#5675));
#1887=EDGE_LOOP('',(#5676));
#1888=EDGE_LOOP('',(#5677));
#1889=EDGE_LOOP('',(#5678));
#1890=EDGE_LOOP('',(#5679));
#1891=EDGE_LOOP('',(#5680));
#1892=EDGE_LOOP('',(#5681));
#1893=EDGE_LOOP('',(#5682,#5683,#5684,#5685));
#1894=EDGE_LOOP('',(#5686,#5687,#5688,#5689));
#1895=EDGE_LOOP('',(#5690,#5691,#5692,#5693));
#1896=EDGE_LOOP('',(#5694,#5695,#5696,#5697));
#1897=EDGE_LOOP('',(#5698,#5699,#5700,#5701));
#1898=EDGE_LOOP('',(#5702,#5703,#5704,#5705));
#1899=EDGE_LOOP('',(#5706));
#1900=EDGE_LOOP('',(#5707));
#1901=EDGE_LOOP('',(#5708));
#1902=EDGE_LOOP('',(#5709));
#1903=EDGE_LOOP('',(#5710));
#1904=EDGE_LOOP('',(#5711));
#1905=EDGE_LOOP('',(#5712));
#1906=EDGE_LOOP('',(#5713));
#1907=EDGE_LOOP('',(#5714));
#1908=EDGE_LOOP('',(#5715));
#1909=EDGE_LOOP('',(#5716));
#1910=EDGE_LOOP('',(#5717));
#1911=EDGE_LOOP('',(#5718,#5719,#5720,#5721));
#1912=EDGE_LOOP('',(#5722,#5723,#5724,#5725));
#1913=EDGE_LOOP('',(#5726));
#1914=EDGE_LOOP('',(#5727));
#1915=EDGE_LOOP('',(#5728));
#1916=EDGE_LOOP('',(#5729));
#1917=EDGE_LOOP('',(#5730,#5731,#5732,#5733));
#1918=EDGE_LOOP('',(#5734,#5735,#5736,#5737));
#1919=EDGE_LOOP('',(#5738,#5739,#5740,#5741));
#1920=EDGE_LOOP('',(#5742,#5743,#5744,#5745));
#1921=EDGE_LOOP('',(#5746,#5747,#5748,#5749));
#1922=EDGE_LOOP('',(#5750,#5751,#5752,#5753));
#1923=EDGE_LOOP('',(#5754));
#1924=EDGE_LOOP('',(#5755));
#1925=EDGE_LOOP('',(#5756));
#1926=EDGE_LOOP('',(#5757));
#1927=EDGE_LOOP('',(#5758));
#1928=EDGE_LOOP('',(#5759));
#1929=EDGE_LOOP('',(#5760));
#1930=EDGE_LOOP('',(#5761));
#1931=EDGE_LOOP('',(#5762));
#1932=EDGE_LOOP('',(#5763));
#1933=EDGE_LOOP('',(#5764));
#1934=EDGE_LOOP('',(#5765));
#1935=EDGE_LOOP('',(#5766,#5767,#5768,#5769));
#1936=EDGE_LOOP('',(#5770,#5771,#5772,#5773));
#1937=EDGE_LOOP('',(#5774,#5775,#5776,#5777));
#1938=EDGE_LOOP('',(#5778,#5779,#5780,#5781));
#1939=EDGE_LOOP('',(#5782,#5783,#5784,#5785));
#1940=EDGE_LOOP('',(#5786,#5787,#5788,#5789));
#1941=EDGE_LOOP('',(#5790));
#1942=EDGE_LOOP('',(#5791));
#1943=EDGE_LOOP('',(#5792));
#1944=EDGE_LOOP('',(#5793));
#1945=EDGE_LOOP('',(#5794));
#1946=EDGE_LOOP('',(#5795));
#1947=EDGE_LOOP('',(#5796));
#1948=EDGE_LOOP('',(#5797));
#1949=EDGE_LOOP('',(#5798));
#1950=EDGE_LOOP('',(#5799));
#1951=EDGE_LOOP('',(#5800));
#1952=EDGE_LOOP('',(#5801));
#1953=EDGE_LOOP('',(#5802,#5803,#5804,#5805));
#1954=EDGE_LOOP('',(#5806,#5807,#5808,#5809));
#1955=EDGE_LOOP('',(#5810,#5811,#5812,#5813));
#1956=EDGE_LOOP('',(#5814));
#1957=EDGE_LOOP('',(#5815,#5816,#5817,#5818));
#1958=EDGE_LOOP('',(#5819,#5820,#5821,#5822));
#1959=EDGE_LOOP('',(#5823));
#1960=EDGE_LOOP('',(#5824,#5825,#5826,#5827));
#1961=EDGE_LOOP('',(#5828,#5829,#5830,#5831));
#1962=EDGE_LOOP('',(#5832,#5833,#5834,#5835));
#1963=EDGE_LOOP('',(#5836,#5837,#5838,#5839));
#1964=EDGE_LOOP('',(#5840,#5841,#5842,#5843));
#1965=EDGE_LOOP('',(#5844,#5845,#5846,#5847));
#1966=EDGE_LOOP('',(#5848,#5849,#5850,#5851));
#1967=EDGE_LOOP('',(#5852,#5853,#5854,#5855));
#1968=EDGE_LOOP('',(#5856,#5857,#5858,#5859));
#1969=EDGE_LOOP('',(#5860,#5861,#5862,#5863));
#1970=EDGE_LOOP('',(#5864,#5865,#5866,#5867));
#1971=EDGE_LOOP('',(#5868,#5869,#5870,#5871));
#1972=EDGE_LOOP('',(#5872,#5873,#5874,#5875));
#1973=EDGE_LOOP('',(#5876,#5877,#5878,#5879));
#1974=EDGE_LOOP('',(#5880,#5881,#5882,#5883));
#1975=EDGE_LOOP('',(#5884));
#1976=EDGE_LOOP('',(#5885));
#1977=EDGE_LOOP('',(#5886));
#1978=EDGE_LOOP('',(#5887));
#1979=EDGE_LOOP('',(#5888));
#1980=EDGE_LOOP('',(#5889));
#1981=EDGE_LOOP('',(#5890));
#1982=EDGE_LOOP('',(#5891));
#1983=EDGE_LOOP('',(#5892));
#1984=EDGE_LOOP('',(#5893));
#1985=EDGE_LOOP('',(#5894,#5895,#5896,#5897));
#1986=EDGE_LOOP('',(#5898,#5899,#5900,#5901));
#1987=EDGE_LOOP('',(#5902,#5903,#5904,#5905));
#1988=EDGE_LOOP('',(#5906));
#1989=EDGE_LOOP('',(#5907));
#1990=EDGE_LOOP('',(#5908));
#1991=EDGE_LOOP('',(#5909));
#1992=EDGE_LOOP('',(#5910));
#1993=EDGE_LOOP('',(#5911));
#1994=EDGE_LOOP('',(#5912));
#1995=EDGE_LOOP('',(#5913));
#1996=EDGE_LOOP('',(#5914));
#1997=EDGE_LOOP('',(#5915));
#1998=EDGE_LOOP('',(#5916,#5917,#5918,#5919));
#1999=EDGE_LOOP('',(#5920,#5921,#5922,#5923));
#2000=EDGE_LOOP('',(#5924));
#2001=EDGE_LOOP('',(#5925));
#2002=EDGE_LOOP('',(#5926));
#2003=EDGE_LOOP('',(#5927));
#2004=EDGE_LOOP('',(#5928,#5929,#5930,#5931));
#2005=EDGE_LOOP('',(#5932,#5933,#5934,#5935));
#2006=EDGE_LOOP('',(#5936,#5937,#5938,#5939));
#2007=EDGE_LOOP('',(#5940,#5941,#5942,#5943));
#2008=EDGE_LOOP('',(#5944,#5945,#5946,#5947));
#2009=EDGE_LOOP('',(#5948,#5949,#5950,#5951));
#2010=EDGE_LOOP('',(#5952));
#2011=EDGE_LOOP('',(#5953));
#2012=EDGE_LOOP('',(#5954));
#2013=EDGE_LOOP('',(#5955));
#2014=EDGE_LOOP('',(#5956));
#2015=EDGE_LOOP('',(#5957));
#2016=EDGE_LOOP('',(#5958));
#2017=EDGE_LOOP('',(#5959));
#2018=EDGE_LOOP('',(#5960));
#2019=EDGE_LOOP('',(#5961));
#2020=EDGE_LOOP('',(#5962));
#2021=EDGE_LOOP('',(#5963));
#2022=EDGE_LOOP('',(#5964,#5965,#5966,#5967));
#2023=EDGE_LOOP('',(#5968,#5969,#5970,#5971));
#2024=EDGE_LOOP('',(#5972,#5973,#5974,#5975));
#2025=EDGE_LOOP('',(#5976,#5977,#5978,#5979));
#2026=EDGE_LOOP('',(#5980,#5981,#5982,#5983));
#2027=EDGE_LOOP('',(#5984,#5985,#5986,#5987));
#2028=EDGE_LOOP('',(#5988));
#2029=EDGE_LOOP('',(#5989));
#2030=EDGE_LOOP('',(#5990));
#2031=EDGE_LOOP('',(#5991));
#2032=EDGE_LOOP('',(#5992));
#2033=EDGE_LOOP('',(#5993));
#2034=EDGE_LOOP('',(#5994));
#2035=EDGE_LOOP('',(#5995));
#2036=EDGE_LOOP('',(#5996));
#2037=EDGE_LOOP('',(#5997));
#2038=EDGE_LOOP('',(#5998));
#2039=EDGE_LOOP('',(#5999));
#2040=EDGE_LOOP('',(#6000,#6001,#6002,#6003));
#2041=EDGE_LOOP('',(#6004,#6005,#6006,#6007));
#2042=EDGE_LOOP('',(#6008));
#2043=EDGE_LOOP('',(#6009));
#2044=EDGE_LOOP('',(#6010));
#2045=EDGE_LOOP('',(#6011));
#2046=EDGE_LOOP('',(#6012,#6013,#6014,#6015));
#2047=EDGE_LOOP('',(#6016,#6017,#6018,#6019));
#2048=EDGE_LOOP('',(#6020,#6021,#6022,#6023));
#2049=EDGE_LOOP('',(#6024,#6025,#6026,#6027));
#2050=EDGE_LOOP('',(#6028,#6029,#6030,#6031));
#2051=EDGE_LOOP('',(#6032,#6033,#6034,#6035));
#2052=EDGE_LOOP('',(#6036));
#2053=EDGE_LOOP('',(#6037));
#2054=EDGE_LOOP('',(#6038));
#2055=EDGE_LOOP('',(#6039));
#2056=EDGE_LOOP('',(#6040));
#2057=EDGE_LOOP('',(#6041));
#2058=EDGE_LOOP('',(#6042));
#2059=EDGE_LOOP('',(#6043));
#2060=EDGE_LOOP('',(#6044));
#2061=EDGE_LOOP('',(#6045));
#2062=EDGE_LOOP('',(#6046));
#2063=EDGE_LOOP('',(#6047));
#2064=EDGE_LOOP('',(#6048,#6049,#6050,#6051));
#2065=EDGE_LOOP('',(#6052,#6053,#6054,#6055));
#2066=EDGE_LOOP('',(#6056,#6057,#6058,#6059));
#2067=EDGE_LOOP('',(#6060,#6061,#6062,#6063));
#2068=EDGE_LOOP('',(#6064,#6065,#6066,#6067));
#2069=EDGE_LOOP('',(#6068,#6069,#6070,#6071));
#2070=EDGE_LOOP('',(#6072));
#2071=EDGE_LOOP('',(#6073));
#2072=EDGE_LOOP('',(#6074));
#2073=EDGE_LOOP('',(#6075));
#2074=EDGE_LOOP('',(#6076));
#2075=EDGE_LOOP('',(#6077));
#2076=EDGE_LOOP('',(#6078));
#2077=EDGE_LOOP('',(#6079));
#2078=EDGE_LOOP('',(#6080));
#2079=EDGE_LOOP('',(#6081));
#2080=EDGE_LOOP('',(#6082));
#2081=EDGE_LOOP('',(#6083));
#2082=EDGE_LOOP('',(#6084,#6085,#6086,#6087,#6088,#6089));
#2083=EDGE_LOOP('',(#6090,#6091,#6092,#6093,#6094));
#2084=EDGE_LOOP('',(#6095,#6096,#6097,#6098));
#2085=EDGE_LOOP('',(#6099,#6100,#6101,#6102));
#2086=EDGE_LOOP('',(#6103));
#2087=EDGE_LOOP('',(#6104));
#2088=EDGE_LOOP('',(#6105,#6106,#6107,#6108,#6109));
#2089=EDGE_LOOP('',(#6110));
#2090=EDGE_LOOP('',(#6111));
#2091=EDGE_LOOP('',(#6112,#6113,#6114,#6115));
#2092=EDGE_LOOP('',(#6116,#6117,#6118,#6119,#6120,#6121));
#2093=EDGE_LOOP('',(#6122,#6123,#6124,#6125,#6126));
#2094=EDGE_LOOP('',(#6127));
#2095=EDGE_LOOP('',(#6128));
#2096=EDGE_LOOP('',(#6129,#6130,#6131,#6132));
#2097=EDGE_LOOP('',(#6133,#6134,#6135,#6136));
#2098=EDGE_LOOP('',(#6137,#6138,#6139,#6140));
#2099=EDGE_LOOP('',(#6141));
#2100=EDGE_LOOP('',(#6142));
#2101=EDGE_LOOP('',(#6143,#6144,#6145,#6146,#6147));
#2102=EDGE_LOOP('',(#6148,#6149));
#2103=EDGE_LOOP('',(#6150,#6151));
#2104=EDGE_LOOP('',(#6152,#6153));
#2105=EDGE_LOOP('',(#6154,#6155));
#2106=EDGE_LOOP('',(#6156,#6157));
#2107=EDGE_LOOP('',(#6158,#6159));
#2108=EDGE_LOOP('',(#6160,#6161));
#2109=EDGE_LOOP('',(#6162,#6163));
#2110=EDGE_LOOP('',(#6164,#6165,#6166,#6167));
#2111=EDGE_LOOP('',(#6168,#6169,#6170,#6171,#6172,#6173,#6174,#6175,#6176,
#6177,#6178,#6179,#6180,#6181,#6182,#6183,#6184,#6185,#6186,#6187));
#2112=EDGE_LOOP('',(#6188,#6189,#6190,#6191));
#2113=EDGE_LOOP('',(#6192,#6193,#6194,#6195));
#2114=EDGE_LOOP('',(#6196,#6197,#6198,#6199));
#2115=EDGE_LOOP('',(#6200,#6201,#6202,#6203));
#2116=EDGE_LOOP('',(#6204,#6205,#6206,#6207));
#2117=EDGE_LOOP('',(#6208,#6209,#6210,#6211,#6212,#6213));
#2118=EDGE_LOOP('',(#6214,#6215,#6216,#6217));
#2119=EDGE_LOOP('',(#6218,#6219,#6220,#6221));
#2120=EDGE_LOOP('',(#6222,#6223,#6224,#6225));
#2121=EDGE_LOOP('',(#6226,#6227,#6228,#6229));
#2122=EDGE_LOOP('',(#6230,#6231,#6232,#6233));
#2123=EDGE_LOOP('',(#6234,#6235,#6236,#6237));
#2124=EDGE_LOOP('',(#6238,#6239,#6240,#6241,#6242,#6243,#6244,#6245,#6246,
#6247,#6248,#6249,#6250,#6251,#6252,#6253,#6254,#6255,#6256,#6257));
#2125=EDGE_LOOP('',(#6258,#6259,#6260,#6261));
#2126=EDGE_LOOP('',(#6262,#6263,#6264,#6265));
#2127=EDGE_LOOP('',(#6266));
#2128=EDGE_LOOP('',(#6267));
#2129=EDGE_LOOP('',(#6268,#6269,#6270,#6271));
#2130=EDGE_LOOP('',(#6272));
#2131=EDGE_LOOP('',(#6273));
#2132=EDGE_LOOP('',(#6274,#6275,#6276,#6277));
#2133=EDGE_LOOP('',(#6278));
#2134=EDGE_LOOP('',(#6279));
#2135=EDGE_LOOP('',(#6280,#6281,#6282,#6283));
#2136=EDGE_LOOP('',(#6284));
#2137=EDGE_LOOP('',(#6285));
#2138=EDGE_LOOP('',(#6286,#6287,#6288,#6289));
#2139=EDGE_LOOP('',(#6290));
#2140=EDGE_LOOP('',(#6291));
#2141=EDGE_LOOP('',(#6292,#6293,#6294,#6295));
#2142=EDGE_LOOP('',(#6296,#6297,#6298,#6299));
#2143=EDGE_LOOP('',(#6300,#6301,#6302,#6303));
#2144=EDGE_LOOP('',(#6304,#6305,#6306,#6307));
#2145=EDGE_LOOP('',(#6308,#6309,#6310,#6311));
#2146=EDGE_LOOP('',(#6312,#6313,#6314,#6315));
#2147=EDGE_LOOP('',(#6316,#6317,#6318,#6319));
#2148=EDGE_LOOP('',(#6320,#6321,#6322,#6323,#6324,#6325));
#2149=EDGE_LOOP('',(#6326,#6327,#6328,#6329,#6330,#6331));
#2150=EDGE_LOOP('',(#6332));
#2151=EDGE_LOOP('',(#6333));
#2152=EDGE_LOOP('',(#6334,#6335,#6336,#6337));
#2153=EDGE_LOOP('',(#6338,#6339,#6340,#6341));
#2154=EDGE_LOOP('',(#6342,#6343,#6344,#6345));
#2155=EDGE_LOOP('',(#6346));
#2156=EDGE_LOOP('',(#6347));
#2157=EDGE_LOOP('',(#6348,#6349,#6350,#6351));
#2158=EDGE_LOOP('',(#6352,#6353,#6354,#6355));
#2159=EDGE_LOOP('',(#6356,#6357,#6358,#6359));
#2160=EDGE_LOOP('',(#6360,#6361,#6362,#6363));
#2161=EDGE_LOOP('',(#6364,#6365,#6366,#6367));
#2162=EDGE_LOOP('',(#6368,#6369,#6370,#6371));
#2163=EDGE_LOOP('',(#6372,#6373,#6374,#6375));
#2164=EDGE_LOOP('',(#6376,#6377,#6378,#6379));
#2165=EDGE_LOOP('',(#6380,#6381,#6382,#6383));
#2166=EDGE_LOOP('',(#6384,#6385,#6386,#6387));
#2167=EDGE_LOOP('',(#6388,#6389,#6390,#6391));
#2168=EDGE_LOOP('',(#6392,#6393,#6394,#6395));
#2169=EDGE_LOOP('',(#6396,#6397,#6398,#6399));
#2170=EDGE_LOOP('',(#6400,#6401,#6402,#6403));
#2171=EDGE_LOOP('',(#6404,#6405,#6406,#6407));
#2172=EDGE_LOOP('',(#6408,#6409,#6410,#6411));
#2173=EDGE_LOOP('',(#6412,#6413,#6414,#6415));
#2174=EDGE_LOOP('',(#6416));
#2175=EDGE_LOOP('',(#6417));
#2176=EDGE_LOOP('',(#6418));
#2177=EDGE_LOOP('',(#6419));
#2178=EDGE_LOOP('',(#6420,#6421,#6422,#6423,#6424,#6425));
#2179=EDGE_LOOP('',(#6426));
#2180=EDGE_LOOP('',(#6427));
#2181=EDGE_LOOP('',(#6428));
#2182=EDGE_LOOP('',(#6429));
#2183=EDGE_LOOP('',(#6430,#6431,#6432,#6433));
#2184=EDGE_LOOP('',(#6434));
#2185=EDGE_LOOP('',(#6435));
#2186=EDGE_LOOP('',(#6436));
#2187=EDGE_LOOP('',(#6437));
#2188=EDGE_LOOP('',(#6438));
#2189=EDGE_LOOP('',(#6439));
#2190=EDGE_LOOP('',(#6440));
#2191=EDGE_LOOP('',(#6441));
#2192=EDGE_LOOP('',(#6442,#6443,#6444,#6445));
#2193=EDGE_LOOP('',(#6446,#6447,#6448,#6449,#6450,#6451));
#2194=EDGE_LOOP('',(#6452));
#2195=EDGE_LOOP('',(#6453));
#2196=EDGE_LOOP('',(#6454));
#2197=EDGE_LOOP('',(#6455));
#2198=EDGE_LOOP('',(#6456));
#2199=EDGE_LOOP('',(#6457));
#2200=EDGE_LOOP('',(#6458));
#2201=EDGE_LOOP('',(#6459));
#2202=EDGE_LOOP('',(#6460,#6461,#6462,#6463,#6464,#6465));
#2203=EDGE_LOOP('',(#6466,#6467,#6468,#6469));
#2204=EDGE_LOOP('',(#6470,#6471,#6472,#6473));
#2205=EDGE_LOOP('',(#6474));
#2206=EDGE_LOOP('',(#6475,#6476,#6477,#6478));
#2207=EDGE_LOOP('',(#6479,#6480,#6481,#6482));
#2208=EDGE_LOOP('',(#6483,#6484,#6485,#6486));
#2209=EDGE_LOOP('',(#6487));
#2210=EDGE_LOOP('',(#6488));
#2211=EDGE_LOOP('',(#6489));
#2212=EDGE_LOOP('',(#6490));
#2213=EDGE_LOOP('',(#6491));
#2214=EDGE_LOOP('',(#6492));
#2215=EDGE_LOOP('',(#6493));
#2216=EDGE_LOOP('',(#6494));
#2217=EDGE_LOOP('',(#6495));
#2218=EDGE_LOOP('',(#6496));
#2219=EDGE_LOOP('',(#6497,#6498,#6499,#6500));
#2220=EDGE_LOOP('',(#6501,#6502,#6503,#6504));
#2221=EDGE_LOOP('',(#6505,#6506,#6507,#6508));
#2222=EDGE_LOOP('',(#6509));
#2223=EDGE_LOOP('',(#6510));
#2224=EDGE_LOOP('',(#6511));
#2225=EDGE_LOOP('',(#6512,#6513,#6514,#6515));
#2226=EDGE_LOOP('',(#6516,#6517,#6518,#6519));
#2227=EDGE_LOOP('',(#6520));
#2228=EDGE_LOOP('',(#6521));
#2229=EDGE_LOOP('',(#6522));
#2230=EDGE_LOOP('',(#6523));
#2231=EDGE_LOOP('',(#6524,#6525,#6526,#6527));
#2232=EDGE_LOOP('',(#6528,#6529,#6530,#6531));
#2233=EDGE_LOOP('',(#6532));
#2234=EDGE_LOOP('',(#6533));
#2235=EDGE_LOOP('',(#6534));
#2236=EDGE_LOOP('',(#6535));
#2237=EDGE_LOOP('',(#6536,#6537,#6538,#6539));
#2238=EDGE_LOOP('',(#6540,#6541,#6542,#6543));
#2239=EDGE_LOOP('',(#6544));
#2240=EDGE_LOOP('',(#6545));
#2241=EDGE_LOOP('',(#6546));
#2242=EDGE_LOOP('',(#6547));
#2243=EDGE_LOOP('',(#6548,#6549,#6550,#6551));
#2244=EDGE_LOOP('',(#6552,#6553,#6554,#6555));
#2245=EDGE_LOOP('',(#6556));
#2246=EDGE_LOOP('',(#6557));
#2247=EDGE_LOOP('',(#6558));
#2248=EDGE_LOOP('',(#6559));
#2249=EDGE_LOOP('',(#6560,#6561,#6562,#6563));
#2250=EDGE_LOOP('',(#6564));
#2251=EDGE_LOOP('',(#6565,#6566,#6567,#6568));
#2252=EDGE_LOOP('',(#6569,#6570,#6571,#6572));
#2253=EDGE_LOOP('',(#6573,#6574,#6575,#6576));
#2254=EDGE_LOOP('',(#6577));
#2255=EDGE_LOOP('',(#6578));
#2256=EDGE_LOOP('',(#6579));
#2257=EDGE_LOOP('',(#6580));
#2258=EDGE_LOOP('',(#6581));
#2259=EDGE_LOOP('',(#6582));
#2260=EDGE_LOOP('',(#6583));
#2261=EDGE_LOOP('',(#6584));
#2262=EDGE_LOOP('',(#6585));
#2263=EDGE_LOOP('',(#6586));
#2264=EDGE_LOOP('',(#6587,#6588,#6589,#6590));
#2265=EDGE_LOOP('',(#6591,#6592,#6593,#6594));
#2266=EDGE_LOOP('',(#6595,#6596,#6597,#6598));
#2267=EDGE_LOOP('',(#6599));
#2268=EDGE_LOOP('',(#6600));
#2269=EDGE_LOOP('',(#6601));
#2270=EDGE_LOOP('',(#6602,#6603,#6604,#6605));
#2271=EDGE_LOOP('',(#6606,#6607,#6608,#6609));
#2272=EDGE_LOOP('',(#6610));
#2273=EDGE_LOOP('',(#6611));
#2274=EDGE_LOOP('',(#6612));
#2275=EDGE_LOOP('',(#6613));
#2276=EDGE_LOOP('',(#6614,#6615,#6616,#6617));
#2277=EDGE_LOOP('',(#6618,#6619,#6620,#6621));
#2278=EDGE_LOOP('',(#6622));
#2279=EDGE_LOOP('',(#6623));
#2280=EDGE_LOOP('',(#6624));
#2281=EDGE_LOOP('',(#6625));
#2282=EDGE_LOOP('',(#6626,#6627,#6628,#6629));
#2283=EDGE_LOOP('',(#6630,#6631,#6632,#6633));
#2284=EDGE_LOOP('',(#6634));
#2285=EDGE_LOOP('',(#6635));
#2286=EDGE_LOOP('',(#6636));
#2287=EDGE_LOOP('',(#6637));
#2288=EDGE_LOOP('',(#6638,#6639,#6640,#6641));
#2289=EDGE_LOOP('',(#6642,#6643,#6644,#6645));
#2290=EDGE_LOOP('',(#6646));
#2291=EDGE_LOOP('',(#6647));
#2292=EDGE_LOOP('',(#6648));
#2293=EDGE_LOOP('',(#6649));
#2294=EDGE_LOOP('',(#6650));
#2295=EDGE_LOOP('',(#6651,#6652,#6653,#6654));
#2296=EDGE_LOOP('',(#6655,#6656,#6657,#6658));
#2297=EDGE_LOOP('',(#6659,#6660,#6661,#6662));
#2298=EDGE_LOOP('',(#6663));
#2299=EDGE_LOOP('',(#6664));
#2300=EDGE_LOOP('',(#6665,#6666,#6667,#6668));
#2301=EDGE_LOOP('',(#6669,#6670,#6671,#6672));
#2302=EDGE_LOOP('',(#6673,#6674,#6675,#6676));
#2303=EDGE_LOOP('',(#6677));
#2304=EDGE_LOOP('',(#6678,#6679,#6680,#6681));
#2305=EDGE_LOOP('',(#6682,#6683,#6684,#6685));
#2306=EDGE_LOOP('',(#6686,#6687,#6688,#6689));
#2307=EDGE_LOOP('',(#6690,#6691,#6692,#6693));
#2308=EDGE_LOOP('',(#6694,#6695,#6696,#6697));
#2309=EDGE_LOOP('',(#6698,#6699,#6700,#6701));
#2310=EDGE_LOOP('',(#6702,#6703,#6704,#6705,#6706,#6707));
#2311=EDGE_LOOP('',(#6708,#6709,#6710,#6711,#6712,#6713));
#2312=LINE('',#11435,#2706);
#2313=LINE('',#11441,#2707);
#2314=LINE('',#11447,#2708);
#2315=LINE('',#11453,#2709);
#2316=LINE('',#11458,#2710);
#2317=LINE('',#11460,#2711);
#2318=LINE('',#11462,#2712);
#2319=LINE('',#11463,#2713);
#2320=LINE('',#11466,#2714);
#2321=LINE('',#11468,#2715);
#2322=LINE('',#11469,#2716);
#2323=LINE('',#11472,#2717);
#2324=LINE('',#11474,#2718);
#2325=LINE('',#11475,#2719);
#2326=LINE('',#11477,#2720);
#2327=LINE('',#11478,#2721);
#2328=LINE('',#11485,#2722);
#2329=LINE('',#11487,#2723);
#2330=LINE('',#11489,#2724);
#2331=LINE('',#11490,#2725);
#2332=LINE('',#11493,#2726);
#2333=LINE('',#11495,#2727);
#2334=LINE('',#11496,#2728);
#2335=LINE('',#11499,#2729);
#2336=LINE('',#11501,#2730);
#2337=LINE('',#11502,#2731);
#2338=LINE('',#11504,#2732);
#2339=LINE('',#11505,#2733);
#2340=LINE('',#11512,#2734);
#2341=LINE('',#11514,#2735);
#2342=LINE('',#11516,#2736);
#2343=LINE('',#11517,#2737);
#2344=LINE('',#11520,#2738);
#2345=LINE('',#11522,#2739);
#2346=LINE('',#11523,#2740);
#2347=LINE('',#11526,#2741);
#2348=LINE('',#11528,#2742);
#2349=LINE('',#11529,#2743);
#2350=LINE('',#11531,#2744);
#2351=LINE('',#11532,#2745);
#2352=LINE('',#11540,#2746);
#2353=LINE('',#11547,#2747);
#2354=LINE('',#11553,#2748);
#2355=LINE('',#11559,#2749);
#2356=LINE('',#11565,#2750);
#2357=LINE('',#11571,#2751);
#2358=LINE('',#11577,#2752);
#2359=LINE('',#11583,#2753);
#2360=LINE('',#11589,#2754);
#2361=LINE('',#11595,#2755);
#2362=LINE('',#11601,#2756);
#2363=LINE('',#11607,#2757);
#2364=LINE('',#11613,#2758);
#2365=LINE('',#11618,#2759);
#2366=LINE('',#11620,#2760);
#2367=LINE('',#11622,#2761);
#2368=LINE('',#11624,#2762);
#2369=LINE('',#11626,#2763);
#2370=LINE('',#11628,#2764);
#2371=LINE('',#11630,#2765);
#2372=LINE('',#11631,#2766);
#2373=LINE('',#11634,#2767);
#2374=LINE('',#11636,#2768);
#2375=LINE('',#11637,#2769);
#2376=LINE('',#11640,#2770);
#2377=LINE('',#11642,#2771);
#2378=LINE('',#11643,#2772);
#2379=LINE('',#11645,#2773);
#2380=LINE('',#11646,#2774);
#2381=LINE('',#11650,#2775);
#2382=LINE('',#11652,#2776);
#2383=LINE('',#11653,#2777);
#2384=LINE('',#11656,#2778);
#2385=LINE('',#11657,#2779);
#2386=LINE('',#11660,#2780);
#2387=LINE('',#11661,#2781);
#2388=LINE('',#11663,#2782);
#2389=LINE('',#11670,#2783);
#2390=LINE('',#11677,#2784);
#2391=LINE('',#11683,#2785);
#2392=LINE('',#11689,#2786);
#2393=LINE('',#11702,#2787);
#2394=LINE('',#11705,#2788);
#2395=LINE('',#11710,#2789);
#2396=LINE('',#11718,#2790);
#2397=LINE('',#11724,#2791);
#2398=LINE('',#11733,#2792);
#2399=LINE('',#11739,#2793);
#2400=LINE('',#11748,#2794);
#2401=LINE('',#11754,#2795);
#2402=LINE('',#11763,#2796);
#2403=LINE('',#11769,#2797);
#2404=LINE('',#11778,#2798);
#2405=LINE('',#11785,#2799);
#2406=LINE('',#11791,#2800);
#2407=LINE('',#11797,#2801);
#2408=LINE('',#11810,#2802);
#2409=LINE('',#11813,#2803);
#2410=LINE('',#11818,#2804);
#2411=LINE('',#11826,#2805);
#2412=LINE('',#11832,#2806);
#2413=LINE('',#11841,#2807);
#2414=LINE('',#11847,#2808);
#2415=LINE('',#11856,#2809);
#2416=LINE('',#11862,#2810);
#2417=LINE('',#11871,#2811);
#2418=LINE('',#11877,#2812);
#2419=LINE('',#11886,#2813);
#2420=LINE('',#11892,#2814);
#2421=LINE('',#11897,#2815);
#2422=LINE('',#11899,#2816);
#2423=LINE('',#11901,#2817);
#2424=LINE('',#11902,#2818);
#2425=LINE('',#11905,#2819);
#2426=LINE('',#11907,#2820);
#2427=LINE('',#11908,#2821);
#2428=LINE('',#11911,#2822);
#2429=LINE('',#11913,#2823);
#2430=LINE('',#11915,#2824);
#2431=LINE('',#11917,#2825);
#2432=LINE('',#11919,#2826);
#2433=LINE('',#11920,#2827);
#2434=LINE('',#11923,#2828);
#2435=LINE('',#11924,#2829);
#2436=LINE('',#11928,#2830);
#2437=LINE('',#11929,#2831);
#2438=LINE('',#11930,#2832);
#2439=LINE('',#11932,#2833);
#2440=LINE('',#11935,#2834);
#2441=LINE('',#11937,#2835);
#2442=LINE('',#11938,#2836);
#2443=LINE('',#11941,#2837);
#2444=LINE('',#11943,#2838);
#2445=LINE('',#11944,#2839);
#2446=LINE('',#11946,#2840);
#2447=LINE('',#11947,#2841);
#2448=LINE('',#11955,#2842);
#2449=LINE('',#11991,#2843);
#2450=LINE('',#11998,#2844);
#2451=LINE('',#12061,#2845);
#2452=LINE('',#12593,#2846);
#2453=LINE('',#12595,#2847);
#2454=LINE('',#12597,#2848);
#2455=LINE('',#12598,#2849);
#2456=LINE('',#12601,#2850);
#2457=LINE('',#12603,#2851);
#2458=LINE('',#12604,#2852);
#2459=LINE('',#12607,#2853);
#2460=LINE('',#12609,#2854);
#2461=LINE('',#12610,#2855);
#2462=LINE('',#12613,#2856);
#2463=LINE('',#12615,#2857);
#2464=LINE('',#12616,#2858);
#2465=LINE('',#12619,#2859);
#2466=LINE('',#12621,#2860);
#2467=LINE('',#12622,#2861);
#2468=LINE('',#12624,#2862);
#2469=LINE('',#12625,#2863);
#2470=LINE('',#12637,#2864);
#2471=LINE('',#12641,#2865);
#2472=LINE('',#12645,#2866);
#2473=LINE('',#12652,#2867);
#2474=LINE('',#12654,#2868);
#2475=LINE('',#12661,#2869);
#2476=LINE('',#12667,#2870);
#2477=LINE('',#12673,#2871);
#2478=LINE('',#12679,#2872);
#2479=LINE('',#12685,#2873);
#2480=LINE('',#12691,#2874);
#2481=LINE('',#12697,#2875);
#2482=LINE('',#12703,#2876);
#2483=LINE('',#12709,#2877);
#2484=LINE('',#12715,#2878);
#2485=LINE('',#12720,#2879);
#2486=LINE('',#12724,#2880);
#2487=LINE('',#12728,#2881);
#2488=LINE('',#12730,#2882);
#2489=LINE('',#12731,#2883);
#2490=LINE('',#12734,#2884);
#2491=LINE('',#12738,#2885);
#2492=LINE('',#12739,#2886);
#2493=LINE('',#12748,#2887);
#2494=LINE('',#12754,#2888);
#2495=LINE('',#12763,#2889);
#2496=LINE('',#12769,#2890);
#2497=LINE('',#12775,#2891);
#2498=LINE('',#12781,#2892);
#2499=LINE('',#12787,#2893);
#2500=LINE('',#12793,#2894);
#2501=LINE('',#12802,#2895);
#2502=LINE('',#12808,#2896);
#2503=LINE('',#12814,#2897);
#2504=LINE('',#12820,#2898);
#2505=LINE('',#12826,#2899);
#2506=LINE('',#12832,#2900);
#2507=LINE('',#12841,#2901);
#2508=LINE('',#12847,#2902);
#2509=LINE('',#12856,#2903);
#2510=LINE('',#12862,#2904);
#2511=LINE('',#12868,#2905);
#2512=LINE('',#12874,#2906);
#2513=LINE('',#12880,#2907);
#2514=LINE('',#12886,#2908);
#2515=LINE('',#12895,#2909);
#2516=LINE('',#12901,#2910);
#2517=LINE('',#12907,#2911);
#2518=LINE('',#12913,#2912);
#2519=LINE('',#12919,#2913);
#2520=LINE('',#12925,#2914);
#2521=LINE('',#12934,#2915);
#2522=LINE('',#12939,#2916);
#2523=LINE('',#12941,#2917);
#2524=LINE('',#12943,#2918);
#2525=LINE('',#12944,#2919);
#2526=LINE('',#12947,#2920);
#2527=LINE('',#12949,#2921);
#2528=LINE('',#12950,#2922);
#2529=LINE('',#12953,#2923);
#2530=LINE('',#12955,#2924);
#2531=LINE('',#12956,#2925);
#2532=LINE('',#12958,#2926);
#2533=LINE('',#12959,#2927);
#2534=LINE('',#12968,#2928);
#2535=LINE('',#12974,#2929);
#2536=LINE('',#12980,#2930);
#2537=LINE('',#12986,#2931);
#2538=LINE('',#12992,#2932);
#2539=LINE('',#12998,#2933);
#2540=LINE('',#13004,#2934);
#2541=LINE('',#13010,#2935);
#2542=LINE('',#13016,#2936);
#2543=LINE('',#13022,#2937);
#2544=LINE('',#13027,#2938);
#2545=LINE('',#13031,#2939);
#2546=LINE('',#13035,#2940);
#2547=LINE('',#13037,#2941);
#2548=LINE('',#13038,#2942);
#2549=LINE('',#13041,#2943);
#2550=LINE('',#13045,#2944);
#2551=LINE('',#13046,#2945);
#2552=LINE('',#13055,#2946);
#2553=LINE('',#13061,#2947);
#2554=LINE('',#13070,#2948);
#2555=LINE('',#13076,#2949);
#2556=LINE('',#13082,#2950);
#2557=LINE('',#13088,#2951);
#2558=LINE('',#13094,#2952);
#2559=LINE('',#13100,#2953);
#2560=LINE('',#13109,#2954);
#2561=LINE('',#13115,#2955);
#2562=LINE('',#13121,#2956);
#2563=LINE('',#13127,#2957);
#2564=LINE('',#13133,#2958);
#2565=LINE('',#13139,#2959);
#2566=LINE('',#13148,#2960);
#2567=LINE('',#13154,#2961);
#2568=LINE('',#13163,#2962);
#2569=LINE('',#13169,#2963);
#2570=LINE('',#13175,#2964);
#2571=LINE('',#13181,#2965);
#2572=LINE('',#13187,#2966);
#2573=LINE('',#13193,#2967);
#2574=LINE('',#13202,#2968);
#2575=LINE('',#13208,#2969);
#2576=LINE('',#13214,#2970);
#2577=LINE('',#13220,#2971);
#2578=LINE('',#13226,#2972);
#2579=LINE('',#13232,#2973);
#2580=LINE('',#13250,#2974);
#2581=LINE('',#13256,#2975);
#2582=LINE('',#13260,#2976);
#2583=LINE('',#13266,#2977);
#2584=LINE('',#13271,#2978);
#2585=LINE('',#13286,#2979);
#2586=LINE('',#13295,#2980);
#2587=LINE('',#13299,#2981);
#2588=LINE('',#13303,#2982);
#2589=LINE('',#13306,#2983);
#2590=LINE('',#13459,#2984);
#2591=LINE('',#13755,#2985);
#2592=LINE('',#13797,#2986);
#2593=LINE('',#13802,#2987);
#2594=LINE('',#13811,#2988);
#2595=LINE('',#13816,#2989);
#2596=LINE('',#13826,#2990);
#2597=LINE('',#13828,#2991);
#2598=LINE('',#13830,#2992);
#2599=LINE('',#13831,#2993);
#2600=LINE('',#13834,#2994);
#2601=LINE('',#13836,#2995);
#2602=LINE('',#13837,#2996);
#2603=LINE('',#13840,#2997);
#2604=LINE('',#13842,#2998);
#2605=LINE('',#13843,#2999);
#2606=LINE('',#13846,#3000);
#2607=LINE('',#13848,#3001);
#2608=LINE('',#13849,#3002);
#2609=LINE('',#13852,#3003);
#2610=LINE('',#13854,#3004);
#2611=LINE('',#13855,#3005);
#2612=LINE('',#13857,#3006);
#2613=LINE('',#13858,#3007);
#2614=LINE('',#13870,#3008);
#2615=LINE('',#13874,#3009);
#2616=LINE('',#13878,#3010);
#2617=LINE('',#13885,#3011);
#2618=LINE('',#13887,#3012);
#2619=LINE('',#13949,#3013);
#2620=LINE('',#13955,#3014);
#2621=LINE('',#13961,#3015);
#2622=LINE('',#13967,#3016);
#2623=LINE('',#13973,#3017);
#2624=LINE('',#13979,#3018);
#2625=LINE('',#13985,#3019);
#2626=LINE('',#13991,#3020);
#2627=LINE('',#13997,#3021);
#2628=LINE('',#14003,#3022);
#2629=LINE('',#14009,#3023);
#2630=LINE('',#14015,#3024);
#2631=LINE('',#14020,#3025);
#2632=LINE('',#14022,#3026);
#2633=LINE('',#14024,#3027);
#2634=LINE('',#14025,#3028);
#2635=LINE('',#14028,#3029);
#2636=LINE('',#14030,#3030);
#2637=LINE('',#14031,#3031);
#2638=LINE('',#14034,#3032);
#2639=LINE('',#14035,#3033);
#2640=LINE('',#14039,#3034);
#2641=LINE('',#14040,#3035);
#2642=LINE('',#14042,#3036);
#2643=LINE('',#14043,#3037);
#2644=LINE('',#14047,#3038);
#2645=LINE('',#14048,#3039);
#2646=LINE('',#14049,#3040);
#2647=LINE('',#14052,#3041);
#2648=LINE('',#14053,#3042);
#2649=LINE('',#14056,#3043);
#2650=LINE('',#14057,#3044);
#2651=LINE('',#14059,#3045);
#2652=LINE('',#14066,#3046);
#2653=LINE('',#14073,#3047);
#2654=LINE('',#14079,#3048);
#2655=LINE('',#14085,#3049);
#2656=LINE('',#14098,#3050);
#2657=LINE('',#14101,#3051);
#2658=LINE('',#14106,#3052);
#2659=LINE('',#14114,#3053);
#2660=LINE('',#14120,#3054);
#2661=LINE('',#14129,#3055);
#2662=LINE('',#14135,#3056);
#2663=LINE('',#14144,#3057);
#2664=LINE('',#14150,#3058);
#2665=LINE('',#14159,#3059);
#2666=LINE('',#14165,#3060);
#2667=LINE('',#14174,#3061);
#2668=LINE('',#14181,#3062);
#2669=LINE('',#14187,#3063);
#2670=LINE('',#14193,#3064);
#2671=LINE('',#14206,#3065);
#2672=LINE('',#14209,#3066);
#2673=LINE('',#14214,#3067);
#2674=LINE('',#14222,#3068);
#2675=LINE('',#14228,#3069);
#2676=LINE('',#14237,#3070);
#2677=LINE('',#14243,#3071);
#2678=LINE('',#14252,#3072);
#2679=LINE('',#14258,#3073);
#2680=LINE('',#14267,#3074);
#2681=LINE('',#14273,#3075);
#2682=LINE('',#14284,#3076);
#2683=LINE('',#14288,#3077);
#2684=LINE('',#14292,#3078);
#2685=LINE('',#14299,#3079);
#2686=LINE('',#14303,#3080);
#2687=LINE('',#14307,#3081);
#2688=LINE('',#14312,#3082);
#2689=LINE('',#14314,#3083);
#2690=LINE('',#14316,#3084);
#2691=LINE('',#14317,#3085);
#2692=LINE('',#14320,#3086);
#2693=LINE('',#14322,#3087);
#2694=LINE('',#14323,#3088);
#2695=LINE('',#14326,#3089);
#2696=LINE('',#14328,#3090);
#2697=LINE('',#14329,#3091);
#2698=LINE('',#14332,#3092);
#2699=LINE('',#14334,#3093);
#2700=LINE('',#14335,#3094);
#2701=LINE('',#14338,#3095);
#2702=LINE('',#14340,#3096);
#2703=LINE('',#14341,#3097);
#2704=LINE('',#14343,#3098);
#2705=LINE('',#14344,#3099);
#2706=VECTOR('',#8980,0.21);
#2707=VECTOR('',#8987,0.21);
#2708=VECTOR('',#8994,0.21);
#2709=VECTOR('',#9001,0.21);
#2710=VECTOR('',#9006,1.);
#2711=VECTOR('',#9007,1.);
#2712=VECTOR('',#9008,1.);
#2713=VECTOR('',#9009,1.);
#2714=VECTOR('',#9012,1.);
#2715=VECTOR('',#9013,1.);
#2716=VECTOR('',#9014,1.);
#2717=VECTOR('',#9017,1.);
#2718=VECTOR('',#9018,1.);
#2719=VECTOR('',#9019,1.);
#2720=VECTOR('',#9022,1.);
#2721=VECTOR('',#9023,1.);
#2722=VECTOR('',#9032,1.);
#2723=VECTOR('',#9033,1.);
#2724=VECTOR('',#9034,1.);
#2725=VECTOR('',#9035,1.);
#2726=VECTOR('',#9038,1.);
#2727=VECTOR('',#9039,1.);
#2728=VECTOR('',#9040,1.);
#2729=VECTOR('',#9043,1.);
#2730=VECTOR('',#9044,1.);
#2731=VECTOR('',#9045,1.);
#2732=VECTOR('',#9048,1.);
#2733=VECTOR('',#9049,1.);
#2734=VECTOR('',#9058,1.);
#2735=VECTOR('',#9059,1.);
#2736=VECTOR('',#9060,1.);
#2737=VECTOR('',#9061,1.);
#2738=VECTOR('',#9064,1.);
#2739=VECTOR('',#9065,1.);
#2740=VECTOR('',#9066,1.);
#2741=VECTOR('',#9069,1.);
#2742=VECTOR('',#9070,1.);
#2743=VECTOR('',#9071,1.);
#2744=VECTOR('',#9074,1.);
#2745=VECTOR('',#9075,1.);
#2746=VECTOR('',#9086,0.164999999999999);
#2747=VECTOR('',#9095,0.165);
#2748=VECTOR('',#9102,0.165);
#2749=VECTOR('',#9109,0.165);
#2750=VECTOR('',#9116,0.505);
#2751=VECTOR('',#9123,0.165);
#2752=VECTOR('',#9130,0.165);
#2753=VECTOR('',#9137,0.165);
#2754=VECTOR('',#9144,0.505);
#2755=VECTOR('',#9151,0.275);
#2756=VECTOR('',#9158,0.275);
#2757=VECTOR('',#9165,0.275);
#2758=VECTOR('',#9172,0.275);
#2759=VECTOR('',#9177,1.);
#2760=VECTOR('',#9178,1.);
#2761=VECTOR('',#9179,1.);
#2762=VECTOR('',#9180,1.);
#2763=VECTOR('',#9181,1.);
#2764=VECTOR('',#9182,1.);
#2765=VECTOR('',#9183,1.);
#2766=VECTOR('',#9184,1.);
#2767=VECTOR('',#9187,1.);
#2768=VECTOR('',#9188,1.);
#2769=VECTOR('',#9189,1.);
#2770=VECTOR('',#9192,1.);
#2771=VECTOR('',#9193,1.);
#2772=VECTOR('',#9194,1.);
#2773=VECTOR('',#9197,1.);
#2774=VECTOR('',#9198,1.);
#2775=VECTOR('',#9203,1.);
#2776=VECTOR('',#9204,1.);
#2777=VECTOR('',#9205,1.);
#2778=VECTOR('',#9208,1.);
#2779=VECTOR('',#9209,1.);
#2780=VECTOR('',#9212,1.);
#2781=VECTOR('',#9213,1.);
#2782=VECTOR('',#9216,1.);
#2783=VECTOR('',#9225,0.165);
#2784=VECTOR('',#9234,0.225);
#2785=VECTOR('',#9241,0.225);
#2786=VECTOR('',#9248,0.225);
#2787=VECTOR('',#9265,1.5);
#2788=VECTOR('',#9268,0.5);
#2789=VECTOR('',#9275,0.5);
#2790=VECTOR('',#9286,0.505);
#2791=VECTOR('',#9293,0.7);
#2792=VECTOR('',#9306,0.505);
#2793=VECTOR('',#9313,0.7);
#2794=VECTOR('',#9326,0.505);
#2795=VECTOR('',#9333,0.7);
#2796=VECTOR('',#9346,0.225);
#2797=VECTOR('',#9353,0.9);
#2798=VECTOR('',#9366,0.165);
#2799=VECTOR('',#9375,0.225);
#2800=VECTOR('',#9382,0.225);
#2801=VECTOR('',#9389,0.225);
#2802=VECTOR('',#9406,1.5);
#2803=VECTOR('',#9409,0.5);
#2804=VECTOR('',#9416,0.5);
#2805=VECTOR('',#9427,0.505);
#2806=VECTOR('',#9434,0.7);
#2807=VECTOR('',#9447,0.505);
#2808=VECTOR('',#9454,0.7);
#2809=VECTOR('',#9467,0.505);
#2810=VECTOR('',#9474,0.7);
#2811=VECTOR('',#9487,0.225);
#2812=VECTOR('',#9494,0.9);
#2813=VECTOR('',#9507,0.225);
#2814=VECTOR('',#9514,0.07);
#2815=VECTOR('',#9519,1.);
#2816=VECTOR('',#9520,1.);
#2817=VECTOR('',#9521,1.);
#2818=VECTOR('',#9522,1.);
#2819=VECTOR('',#9525,1.);
#2820=VECTOR('',#9526,1.);
#2821=VECTOR('',#9527,1.);
#2822=VECTOR('',#9530,1.);
#2823=VECTOR('',#9531,1.);
#2824=VECTOR('',#9532,1.);
#2825=VECTOR('',#9533,1.);
#2826=VECTOR('',#9534,1.);
#2827=VECTOR('',#9535,1.);
#2828=VECTOR('',#9538,1.);
#2829=VECTOR('',#9539,1.);
#2830=VECTOR('',#9542,1.);
#2831=VECTOR('',#9543,1.);
#2832=VECTOR('',#9544,1.);
#2833=VECTOR('',#9547,1.);
#2834=VECTOR('',#9550,1.);
#2835=VECTOR('',#9551,1.);
#2836=VECTOR('',#9552,1.);
#2837=VECTOR('',#9555,1.);
#2838=VECTOR('',#9556,1.);
#2839=VECTOR('',#9557,1.);
#2840=VECTOR('',#9560,1.);
#2841=VECTOR('',#9561,1.);
#2842=VECTOR('',#9572,0.0599999999999996);
#2843=VECTOR('',#9581,1.);
#2844=VECTOR('',#9590,0.0600000000000001);
#2845=VECTOR('',#9597,1.);
#2846=VECTOR('',#9606,1.);
#2847=VECTOR('',#9607,1.);
#2848=VECTOR('',#9608,1.);
#2849=VECTOR('',#9609,1.);
#2850=VECTOR('',#9612,1.);
#2851=VECTOR('',#9613,1.);
#2852=VECTOR('',#9614,1.);
#2853=VECTOR('',#9617,1.);
#2854=VECTOR('',#9618,1.);
#2855=VECTOR('',#9619,1.);
#2856=VECTOR('',#9622,1.);
#2857=VECTOR('',#9623,1.);
#2858=VECTOR('',#9624,1.);
#2859=VECTOR('',#9627,1.);
#2860=VECTOR('',#9628,1.);
#2861=VECTOR('',#9629,1.);
#2862=VECTOR('',#9632,1.);
#2863=VECTOR('',#9633,1.);
#2864=VECTOR('',#9650,0.4);
#2865=VECTOR('',#9655,0.425);
#2866=VECTOR('',#9660,0.41);
#2867=VECTOR('',#9669,0.26);
#2868=VECTOR('',#9672,0.25);
#2869=VECTOR('',#9681,0.164999999999999);
#2870=VECTOR('',#9688,0.164999999999999);
#2871=VECTOR('',#9695,0.164999999999999);
#2872=VECTOR('',#9702,0.164999999999999);
#2873=VECTOR('',#9709,0.165);
#2874=VECTOR('',#9716,0.165);
#2875=VECTOR('',#9723,0.165);
#2876=VECTOR('',#9730,0.165);
#2877=VECTOR('',#9737,1.5);
#2878=VECTOR('',#9744,1.5);
#2879=VECTOR('',#9749,1.);
#2880=VECTOR('',#9752,1.);
#2881=VECTOR('',#9757,1.);
#2882=VECTOR('',#9758,1.);
#2883=VECTOR('',#9759,1.);
#2884=VECTOR('',#9762,1.);
#2885=VECTOR('',#9767,1.);
#2886=VECTOR('',#9768,1.);
#2887=VECTOR('',#9781,1.02);
#2888=VECTOR('',#9788,1.49);
#2889=VECTOR('',#9801,0.225);
#2890=VECTOR('',#9808,0.225);
#2891=VECTOR('',#9815,0.225);
#2892=VECTOR('',#9822,0.225);
#2893=VECTOR('',#9829,1.02);
#2894=VECTOR('',#9836,2.2);
#2895=VECTOR('',#9849,0.225);
#2896=VECTOR('',#9856,0.225);
#2897=VECTOR('',#9863,0.225);
#2898=VECTOR('',#9870,0.225);
#2899=VECTOR('',#9877,1.02);
#2900=VECTOR('',#9884,2.2);
#2901=VECTOR('',#9897,1.02);
#2902=VECTOR('',#9904,1.49);
#2903=VECTOR('',#9917,0.225000000000001);
#2904=VECTOR('',#9924,0.225000000000001);
#2905=VECTOR('',#9931,0.225000000000001);
#2906=VECTOR('',#9938,0.225000000000001);
#2907=VECTOR('',#9945,1.02);
#2908=VECTOR('',#9952,2.2);
#2909=VECTOR('',#9965,0.225000000000001);
#2910=VECTOR('',#9972,0.225000000000001);
#2911=VECTOR('',#9979,0.225000000000001);
#2912=VECTOR('',#9986,0.225000000000001);
#2913=VECTOR('',#9993,1.02);
#2914=VECTOR('',#10000,2.2);
#2915=VECTOR('',#10013,0.0700000000000003);
#2916=VECTOR('',#10018,1.);
#2917=VECTOR('',#10019,1.);
#2918=VECTOR('',#10020,1.);
#2919=VECTOR('',#10021,1.);
#2920=VECTOR('',#10024,1.);
#2921=VECTOR('',#10025,1.);
#2922=VECTOR('',#10026,1.);
#2923=VECTOR('',#10029,1.);
#2924=VECTOR('',#10030,1.);
#2925=VECTOR('',#10031,1.);
#2926=VECTOR('',#10034,1.);
#2927=VECTOR('',#10035,1.);
#2928=VECTOR('',#10048,0.164999999999999);
#2929=VECTOR('',#10055,0.164999999999999);
#2930=VECTOR('',#10062,0.164999999999999);
#2931=VECTOR('',#10069,0.164999999999999);
#2932=VECTOR('',#10076,0.165);
#2933=VECTOR('',#10083,0.165);
#2934=VECTOR('',#10090,0.165);
#2935=VECTOR('',#10097,0.165);
#2936=VECTOR('',#10104,1.5);
#2937=VECTOR('',#10111,1.5);
#2938=VECTOR('',#10116,1.);
#2939=VECTOR('',#10119,1.);
#2940=VECTOR('',#10124,1.);
#2941=VECTOR('',#10125,1.);
#2942=VECTOR('',#10126,1.);
#2943=VECTOR('',#10129,1.);
#2944=VECTOR('',#10134,1.);
#2945=VECTOR('',#10135,1.);
#2946=VECTOR('',#10148,1.02);
#2947=VECTOR('',#10155,1.49);
#2948=VECTOR('',#10168,0.225);
#2949=VECTOR('',#10175,0.225);
#2950=VECTOR('',#10182,0.225);
#2951=VECTOR('',#10189,0.225);
#2952=VECTOR('',#10196,1.02);
#2953=VECTOR('',#10203,2.2);
#2954=VECTOR('',#10216,0.225);
#2955=VECTOR('',#10223,0.225);
#2956=VECTOR('',#10230,0.225);
#2957=VECTOR('',#10237,0.225);
#2958=VECTOR('',#10244,1.02);
#2959=VECTOR('',#10251,2.2);
#2960=VECTOR('',#10264,1.02);
#2961=VECTOR('',#10271,1.49);
#2962=VECTOR('',#10284,0.225000000000001);
#2963=VECTOR('',#10291,0.225000000000001);
#2964=VECTOR('',#10298,0.225000000000001);
#2965=VECTOR('',#10305,0.225000000000001);
#2966=VECTOR('',#10312,1.02);
#2967=VECTOR('',#10319,2.2);
#2968=VECTOR('',#10332,0.225000000000001);
#2969=VECTOR('',#10339,0.225000000000001);
#2970=VECTOR('',#10346,0.225000000000001);
#2971=VECTOR('',#10353,0.225000000000001);
#2972=VECTOR('',#10360,1.02);
#2973=VECTOR('',#10367,2.2);
#2974=VECTOR('',#10392,0.976185);
#2975=VECTOR('',#10399,0.5);
#2976=VECTOR('',#10404,0.53);
#2977=VECTOR('',#10413,0.976185);
#2978=VECTOR('',#10420,0.53);
#2979=VECTOR('',#10439,1.023815);
#2980=VECTOR('',#10450,1.47);
#2981=VECTOR('',#10455,1.5);
#2982=VECTOR('',#10460,1.47);
#2983=VECTOR('',#10465,1.023815);
#2984=VECTOR('',#10516,1.019052);
#2985=VECTOR('',#10593,0.980948);
#2986=VECTOR('',#10622,1.013815);
#2987=VECTOR('',#10629,0.991185);
#2988=VECTOR('',#10640,1.013815);
#2989=VECTOR('',#10647,0.991185);
#2990=VECTOR('',#10662,1.);
#2991=VECTOR('',#10663,1.);
#2992=VECTOR('',#10664,1.);
#2993=VECTOR('',#10665,1.);
#2994=VECTOR('',#10668,1.);
#2995=VECTOR('',#10669,1.);
#2996=VECTOR('',#10670,1.);
#2997=VECTOR('',#10673,1.);
#2998=VECTOR('',#10674,1.);
#2999=VECTOR('',#10675,1.);
#3000=VECTOR('',#10678,1.);
#3001=VECTOR('',#10679,1.);
#3002=VECTOR('',#10680,1.);
#3003=VECTOR('',#10683,1.);
#3004=VECTOR('',#10684,1.);
#3005=VECTOR('',#10685,1.);
#3006=VECTOR('',#10688,1.);
#3007=VECTOR('',#10689,1.);
#3008=VECTOR('',#10706,0.325);
#3009=VECTOR('',#10711,0.35);
#3010=VECTOR('',#10716,0.335);
#3011=VECTOR('',#10725,0.21);
#3012=VECTOR('',#10728,0.2);
#3013=VECTOR('',#10847,0.164999999999999);
#3014=VECTOR('',#10854,0.164999999999999);
#3015=VECTOR('',#10861,0.164999999999999);
#3016=VECTOR('',#10868,0.504999999999999);
#3017=VECTOR('',#10875,0.164999999999999);
#3018=VECTOR('',#10882,0.164999999999999);
#3019=VECTOR('',#10889,0.164999999999999);
#3020=VECTOR('',#10896,0.504999999999999);
#3021=VECTOR('',#10903,0.329999999999998);
#3022=VECTOR('',#10910,0.329999999999998);
#3023=VECTOR('',#10917,0.329999999999998);
#3024=VECTOR('',#10924,0.329999999999998);
#3025=VECTOR('',#10929,1.);
#3026=VECTOR('',#10930,1.);
#3027=VECTOR('',#10931,1.);
#3028=VECTOR('',#10932,1.);
#3029=VECTOR('',#10935,1.);
#3030=VECTOR('',#10936,1.);
#3031=VECTOR('',#10937,1.);
#3032=VECTOR('',#10940,1.);
#3033=VECTOR('',#10941,1.);
#3034=VECTOR('',#10944,1.);
#3035=VECTOR('',#10945,1.);
#3036=VECTOR('',#10946,1.);
#3037=VECTOR('',#10947,1.);
#3038=VECTOR('',#10950,1.);
#3039=VECTOR('',#10951,1.);
#3040=VECTOR('',#10952,1.);
#3041=VECTOR('',#10955,1.);
#3042=VECTOR('',#10956,1.);
#3043=VECTOR('',#10959,1.);
#3044=VECTOR('',#10960,1.);
#3045=VECTOR('',#10963,1.);
#3046=VECTOR('',#10972,0.164999999999999);
#3047=VECTOR('',#10981,0.225000000000001);
#3048=VECTOR('',#10988,0.225000000000001);
#3049=VECTOR('',#10995,0.225000000000001);
#3050=VECTOR('',#11012,1.5);
#3051=VECTOR('',#11015,0.5);
#3052=VECTOR('',#11022,0.5);
#3053=VECTOR('',#11033,0.504999999999999);
#3054=VECTOR('',#11040,0.699999999999999);
#3055=VECTOR('',#11053,0.504999999999999);
#3056=VECTOR('',#11060,0.699999999999999);
#3057=VECTOR('',#11073,0.504999999999999);
#3058=VECTOR('',#11080,0.699999999999999);
#3059=VECTOR('',#11093,0.225000000000001);
#3060=VECTOR('',#11100,0.899999999999999);
#3061=VECTOR('',#11113,0.164999999999999);
#3062=VECTOR('',#11122,0.225000000000001);
#3063=VECTOR('',#11129,0.225000000000001);
#3064=VECTOR('',#11136,0.225000000000001);
#3065=VECTOR('',#11153,1.5);
#3066=VECTOR('',#11156,0.5);
#3067=VECTOR('',#11163,0.5);
#3068=VECTOR('',#11174,0.504999999999999);
#3069=VECTOR('',#11181,0.699999999999999);
#3070=VECTOR('',#11194,0.504999999999999);
#3071=VECTOR('',#11201,0.699999999999999);
#3072=VECTOR('',#11214,0.504999999999999);
#3073=VECTOR('',#11221,0.699999999999999);
#3074=VECTOR('',#11234,0.225000000000001);
#3075=VECTOR('',#11241,0.899999999999999);
#3076=VECTOR('',#11258,0.325);
#3077=VECTOR('',#11263,0.35);
#3078=VECTOR('',#11268,0.335);
#3079=VECTOR('',#11277,0.21);
#3080=VECTOR('',#11282,0.2);
#3081=VECTOR('',#11287,0.18);
#3082=VECTOR('',#11292,1.);
#3083=VECTOR('',#11293,1.);
#3084=VECTOR('',#11294,1.);
#3085=VECTOR('',#11295,1.);
#3086=VECTOR('',#11298,1.);
#3087=VECTOR('',#11299,1.);
#3088=VECTOR('',#11300,1.);
#3089=VECTOR('',#11303,1.);
#3090=VECTOR('',#11304,1.);
#3091=VECTOR('',#11305,1.);
#3092=VECTOR('',#11308,1.);
#3093=VECTOR('',#11309,1.);
#3094=VECTOR('',#11310,1.);
#3095=VECTOR('',#11313,1.);
#3096=VECTOR('',#11314,1.);
#3097=VECTOR('',#11315,1.);
#3098=VECTOR('',#11318,1.);
#3099=VECTOR('',#11319,1.);
#3100=CIRCLE('',#7942,0.21);
#3101=CIRCLE('',#7943,0.21);
#3102=CIRCLE('',#7945,0.21);
#3103=CIRCLE('',#7946,0.21);
#3104=CIRCLE('',#7948,0.21);
#3105=CIRCLE('',#7949,0.21);
#3106=CIRCLE('',#7951,0.21);
#3107=CIRCLE('',#7952,0.21);
#3108=CIRCLE('',#7975,0.164999999999999);
#3109=CIRCLE('',#7976,0.164999999999999);
#3110=CIRCLE('',#7979,0.165);
#3111=CIRCLE('',#7980,0.165);
#3112=CIRCLE('',#7982,0.165);
#3113=CIRCLE('',#7983,0.165);
#3114=CIRCLE('',#7985,0.165);
#3115=CIRCLE('',#7986,0.165);
#3116=CIRCLE('',#7988,0.505);
#3117=CIRCLE('',#7989,0.505);
#3118=CIRCLE('',#7991,0.165);
#3119=CIRCLE('',#7992,0.165);
#3120=CIRCLE('',#7994,0.165);
#3121=CIRCLE('',#7995,0.165);
#3122=CIRCLE('',#7997,0.165);
#3123=CIRCLE('',#7998,0.165);
#3124=CIRCLE('',#8000,0.505);
#3125=CIRCLE('',#8001,0.505);
#3126=CIRCLE('',#8003,0.275);
#3127=CIRCLE('',#8004,0.275);
#3128=CIRCLE('',#8006,0.275);
#3129=CIRCLE('',#8007,0.275);
#3130=CIRCLE('',#8009,0.275);
#3131=CIRCLE('',#8010,0.275);
#3132=CIRCLE('',#8012,0.275);
#3133=CIRCLE('',#8013,0.275);
#3134=CIRCLE('',#8026,0.165);
#3135=CIRCLE('',#8027,0.165);
#3136=CIRCLE('',#8030,0.225);
#3137=CIRCLE('',#8031,0.225);
#3138=CIRCLE('',#8033,0.225);
#3139=CIRCLE('',#8034,0.225);
#3140=CIRCLE('',#8036,0.225);
#3141=CIRCLE('',#8037,0.225);
#3142=CIRCLE('',#8039,1.5);
#3143=CIRCLE('',#8040,0.5);
#3144=CIRCLE('',#8042,1.5);
#3145=CIRCLE('',#8043,0.5);
#3146=CIRCLE('',#8046,0.5);
#3147=CIRCLE('',#8048,0.5);
#3148=CIRCLE('',#8053,0.505);
#3149=CIRCLE('',#8054,0.505);
#3150=CIRCLE('',#8056,0.7);
#3151=CIRCLE('',#8057,0.7);
#3152=CIRCLE('',#8062,0.505);
#3153=CIRCLE('',#8063,0.505);
#3154=CIRCLE('',#8065,0.7);
#3155=CIRCLE('',#8066,0.7);
#3156=CIRCLE('',#8071,0.505);
#3157=CIRCLE('',#8072,0.505);
#3158=CIRCLE('',#8074,0.7);
#3159=CIRCLE('',#8075,0.7);
#3160=CIRCLE('',#8080,0.225);
#3161=CIRCLE('',#8081,0.225);
#3162=CIRCLE('',#8083,0.9);
#3163=CIRCLE('',#8084,0.9);
#3164=CIRCLE('',#8089,0.165);
#3165=CIRCLE('',#8090,0.165);
#3166=CIRCLE('',#8093,0.225);
#3167=CIRCLE('',#8094,0.225);
#3168=CIRCLE('',#8096,0.225);
#3169=CIRCLE('',#8097,0.225);
#3170=CIRCLE('',#8099,0.225);
#3171=CIRCLE('',#8100,0.225);
#3172=CIRCLE('',#8102,1.5);
#3173=CIRCLE('',#8103,0.5);
#3174=CIRCLE('',#8105,1.5);
#3175=CIRCLE('',#8106,0.5);
#3176=CIRCLE('',#8109,0.5);
#3177=CIRCLE('',#8111,0.5);
#3178=CIRCLE('',#8116,0.505);
#3179=CIRCLE('',#8117,0.505);
#3180=CIRCLE('',#8119,0.7);
#3181=CIRCLE('',#8120,0.7);
#3182=CIRCLE('',#8125,0.505);
#3183=CIRCLE('',#8126,0.505);
#3184=CIRCLE('',#8128,0.7);
#3185=CIRCLE('',#8129,0.7);
#3186=CIRCLE('',#8134,0.505);
#3187=CIRCLE('',#8135,0.505);
#3188=CIRCLE('',#8137,0.7);
#3189=CIRCLE('',#8138,0.7);
#3190=CIRCLE('',#8143,0.225);
#3191=CIRCLE('',#8144,0.225);
#3192=CIRCLE('',#8146,0.9);
#3193=CIRCLE('',#8147,0.9);
#3194=CIRCLE('',#8152,0.225);
#3195=CIRCLE('',#8153,0.225);
#3196=CIRCLE('',#8155,0.07);
#3197=CIRCLE('',#8156,0.07);
#3198=CIRCLE('',#8170,0.0599999999999996);
#3199=CIRCLE('',#8171,0.0599999999999996);
#3200=CIRCLE('',#8172,0.0599999999999996);
#3201=CIRCLE('',#8176,0.06);
#3202=CIRCLE('',#8178,0.0600000000000001);
#3203=CIRCLE('',#8179,0.0600000000000001);
#3204=CIRCLE('',#8183,0.06);
#3205=CIRCLE('',#8194,0.24505);
#3206=CIRCLE('',#8196,0.375);
#3207=CIRCLE('',#8198,0.425);
#3208=CIRCLE('',#8200,0.425);
#3209=CIRCLE('',#8202,0.395);
#3210=CIRCLE('',#8204,0.27);
#3211=CIRCLE('',#8206,0.24505);
#3212=CIRCLE('',#8211,0.164999999999999);
#3213=CIRCLE('',#8212,0.164999999999999);
#3214=CIRCLE('',#8214,0.164999999999999);
#3215=CIRCLE('',#8215,0.164999999999999);
#3216=CIRCLE('',#8217,0.164999999999999);
#3217=CIRCLE('',#8218,0.164999999999999);
#3218=CIRCLE('',#8220,0.164999999999999);
#3219=CIRCLE('',#8221,0.164999999999999);
#3220=CIRCLE('',#8223,0.165);
#3221=CIRCLE('',#8224,0.165);
#3222=CIRCLE('',#8226,0.165);
#3223=CIRCLE('',#8227,0.165);
#3224=CIRCLE('',#8229,0.165);
#3225=CIRCLE('',#8230,0.165);
#3226=CIRCLE('',#8232,0.165);
#3227=CIRCLE('',#8233,0.165);
#3228=CIRCLE('',#8235,1.5);
#3229=CIRCLE('',#8236,1.5);
#3230=CIRCLE('',#8238,1.5);
#3231=CIRCLE('',#8239,1.5);
#3232=CIRCLE('',#8241,2.2);
#3233=CIRCLE('',#8242,2.2);
#3234=CIRCLE('',#8245,2.2);
#3235=CIRCLE('',#8248,2.2);
#3236=CIRCLE('',#8252,1.02);
#3237=CIRCLE('',#8253,1.02);
#3238=CIRCLE('',#8255,1.49);
#3239=CIRCLE('',#8256,1.49);
#3240=CIRCLE('',#8261,0.225);
#3241=CIRCLE('',#8262,0.225);
#3242=CIRCLE('',#8264,0.225);
#3243=CIRCLE('',#8265,0.225);
#3244=CIRCLE('',#8267,0.225);
#3245=CIRCLE('',#8268,0.225);
#3246=CIRCLE('',#8270,0.225);
#3247=CIRCLE('',#8271,0.225);
#3248=CIRCLE('',#8273,1.02);
#3249=CIRCLE('',#8274,1.02);
#3250=CIRCLE('',#8276,2.2);
#3251=CIRCLE('',#8277,2.2);
#3252=CIRCLE('',#8282,0.225);
#3253=CIRCLE('',#8283,0.225);
#3254=CIRCLE('',#8285,0.225);
#3255=CIRCLE('',#8286,0.225);
#3256=CIRCLE('',#8288,0.225);
#3257=CIRCLE('',#8289,0.225);
#3258=CIRCLE('',#8291,0.225);
#3259=CIRCLE('',#8292,0.225);
#3260=CIRCLE('',#8294,1.02);
#3261=CIRCLE('',#8295,1.02);
#3262=CIRCLE('',#8297,2.2);
#3263=CIRCLE('',#8298,2.2);
#3264=CIRCLE('',#8303,1.02);
#3265=CIRCLE('',#8304,1.02);
#3266=CIRCLE('',#8306,1.49);
#3267=CIRCLE('',#8307,1.49);
#3268=CIRCLE('',#8312,0.225000000000001);
#3269=CIRCLE('',#8313,0.225000000000001);
#3270=CIRCLE('',#8315,0.225000000000001);
#3271=CIRCLE('',#8316,0.225000000000001);
#3272=CIRCLE('',#8318,0.225000000000001);
#3273=CIRCLE('',#8319,0.225000000000001);
#3274=CIRCLE('',#8321,0.225000000000001);
#3275=CIRCLE('',#8322,0.225000000000001);
#3276=CIRCLE('',#8324,1.02);
#3277=CIRCLE('',#8325,1.02);
#3278=CIRCLE('',#8327,2.2);
#3279=CIRCLE('',#8328,2.2);
#3280=CIRCLE('',#8333,0.225000000000001);
#3281=CIRCLE('',#8334,0.225000000000001);
#3282=CIRCLE('',#8336,0.225000000000001);
#3283=CIRCLE('',#8337,0.225000000000001);
#3284=CIRCLE('',#8339,0.225000000000001);
#3285=CIRCLE('',#8340,0.225000000000001);
#3286=CIRCLE('',#8342,0.225000000000001);
#3287=CIRCLE('',#8343,0.225000000000001);
#3288=CIRCLE('',#8345,1.02);
#3289=CIRCLE('',#8346,1.02);
#3290=CIRCLE('',#8348,2.2);
#3291=CIRCLE('',#8349,2.2);
#3292=CIRCLE('',#8354,0.0700000000000003);
#3293=CIRCLE('',#8355,0.0700000000000003);
#3294=CIRCLE('',#8365,0.164999999999999);
#3295=CIRCLE('',#8366,0.164999999999999);
#3296=CIRCLE('',#8368,0.164999999999999);
#3297=CIRCLE('',#8369,0.164999999999999);
#3298=CIRCLE('',#8371,0.164999999999999);
#3299=CIRCLE('',#8372,0.164999999999999);
#3300=CIRCLE('',#8374,0.164999999999999);
#3301=CIRCLE('',#8375,0.164999999999999);
#3302=CIRCLE('',#8377,0.165);
#3303=CIRCLE('',#8378,0.165);
#3304=CIRCLE('',#8380,0.165);
#3305=CIRCLE('',#8381,0.165);
#3306=CIRCLE('',#8383,0.165);
#3307=CIRCLE('',#8384,0.165);
#3308=CIRCLE('',#8386,0.165);
#3309=CIRCLE('',#8387,0.165);
#3310=CIRCLE('',#8389,1.5);
#3311=CIRCLE('',#8390,1.5);
#3312=CIRCLE('',#8392,1.5);
#3313=CIRCLE('',#8393,1.5);
#3314=CIRCLE('',#8395,2.2);
#3315=CIRCLE('',#8396,2.2);
#3316=CIRCLE('',#8399,2.2);
#3317=CIRCLE('',#8402,2.2);
#3318=CIRCLE('',#8406,1.02);
#3319=CIRCLE('',#8407,1.02);
#3320=CIRCLE('',#8409,1.49);
#3321=CIRCLE('',#8410,1.49);
#3322=CIRCLE('',#8415,0.225);
#3323=CIRCLE('',#8416,0.225);
#3324=CIRCLE('',#8418,0.225);
#3325=CIRCLE('',#8419,0.225);
#3326=CIRCLE('',#8421,0.225);
#3327=CIRCLE('',#8422,0.225);
#3328=CIRCLE('',#8424,0.225);
#3329=CIRCLE('',#8425,0.225);
#3330=CIRCLE('',#8427,1.02);
#3331=CIRCLE('',#8428,1.02);
#3332=CIRCLE('',#8430,2.2);
#3333=CIRCLE('',#8431,2.2);
#3334=CIRCLE('',#8436,0.225);
#3335=CIRCLE('',#8437,0.225);
#3336=CIRCLE('',#8439,0.225);
#3337=CIRCLE('',#8440,0.225);
#3338=CIRCLE('',#8442,0.225);
#3339=CIRCLE('',#8443,0.225);
#3340=CIRCLE('',#8445,0.225);
#3341=CIRCLE('',#8446,0.225);
#3342=CIRCLE('',#8448,1.02);
#3343=CIRCLE('',#8449,1.02);
#3344=CIRCLE('',#8451,2.2);
#3345=CIRCLE('',#8452,2.2);
#3346=CIRCLE('',#8457,1.02);
#3347=CIRCLE('',#8458,1.02);
#3348=CIRCLE('',#8460,1.49);
#3349=CIRCLE('',#8461,1.49);
#3350=CIRCLE('',#8466,0.225000000000001);
#3351=CIRCLE('',#8467,0.225000000000001);
#3352=CIRCLE('',#8469,0.225000000000001);
#3353=CIRCLE('',#8470,0.225000000000001);
#3354=CIRCLE('',#8472,0.225000000000001);
#3355=CIRCLE('',#8473,0.225000000000001);
#3356=CIRCLE('',#8475,0.225000000000001);
#3357=CIRCLE('',#8476,0.225000000000001);
#3358=CIRCLE('',#8478,1.02);
#3359=CIRCLE('',#8479,1.02);
#3360=CIRCLE('',#8481,2.2);
#3361=CIRCLE('',#8482,2.2);
#3362=CIRCLE('',#8487,0.225000000000001);
#3363=CIRCLE('',#8488,0.225000000000001);
#3364=CIRCLE('',#8490,0.225000000000001);
#3365=CIRCLE('',#8491,0.225000000000001);
#3366=CIRCLE('',#8493,0.225000000000001);
#3367=CIRCLE('',#8494,0.225000000000001);
#3368=CIRCLE('',#8496,0.225000000000001);
#3369=CIRCLE('',#8497,0.225000000000001);
#3370=CIRCLE('',#8499,1.02);
#3371=CIRCLE('',#8500,1.02);
#3372=CIRCLE('',#8502,2.2);
#3373=CIRCLE('',#8503,2.2);
#3374=CIRCLE('',#8509,0.976185);
#3375=CIRCLE('',#8510,0.976185);
#3376=CIRCLE('',#8511,0.247676);
#3377=CIRCLE('',#8512,0.976185);
#3378=CIRCLE('',#8513,0.976185);
#3379=CIRCLE('',#8515,0.976185);
#3380=CIRCLE('',#8517,0.5);
#3381=CIRCLE('',#8518,0.5);
#3382=CIRCLE('',#8520,0.56);
#3383=CIRCLE('',#8523,0.976185);
#3384=CIRCLE('',#8525,0.56);
#3385=CIRCLE('',#8529,1.023815);
#3386=CIRCLE('',#8530,1.023815);
#3387=CIRCLE('',#8531,0.247676);
#3388=CIRCLE('',#8532,1.023815);
#3389=CIRCLE('',#8533,1.023815);
#3390=CIRCLE('',#8535,1.023815);
#3391=CIRCLE('',#8537,1.44);
#3392=CIRCLE('',#8538,1.023815);
#3393=CIRCLE('',#8540,1.5);
#3394=CIRCLE('',#8542,1.5);
#3395=CIRCLE('',#8544,1.44);
#3396=CIRCLE('',#8549,0.23815);
#3397=CIRCLE('',#8551,0.23815);
#3398=CIRCLE('',#8553,0.23815);
#3399=CIRCLE('',#8555,0.23815);
#3400=CIRCLE('',#8557,0.23815);
#3401=CIRCLE('',#8559,0.23815);
#3402=CIRCLE('',#8561,0.23815);
#3403=CIRCLE('',#8563,0.23815);
#3404=CIRCLE('',#8566,0.243053047864041);
#3405=CIRCLE('',#8567,0.243053047864041);
#3406=CIRCLE('',#8569,1.019052);
#3407=CIRCLE('',#8570,1.019052);
#3408=CIRCLE('',#8571,1.019052);
#3409=CIRCLE('',#8572,1.019052);
#3410=CIRCLE('',#8573,1.019052);
#3411=CIRCLE('',#8574,1.019052);
#3412=CIRCLE('',#8575,1.019052);
#3413=CIRCLE('',#8576,1.019052);
#3414=CIRCLE('',#8577,1.019052);
#3415=CIRCLE('',#8579,0.980948);
#3416=CIRCLE('',#8580,0.243053047864041);
#3417=CIRCLE('',#8582,0.243053047864041);
#3418=CIRCLE('',#8584,0.980948);
#3419=CIRCLE('',#8585,0.243053047864041);
#3420=CIRCLE('',#8587,0.243053047864041);
#3421=CIRCLE('',#8589,0.980948);
#3422=CIRCLE('',#8590,0.243053047864041);
#3423=CIRCLE('',#8592,0.243053047864041);
#3424=CIRCLE('',#8594,0.980948);
#3425=CIRCLE('',#8595,0.243053047864041);
#3426=CIRCLE('',#8597,0.243053047864041);
#3427=CIRCLE('',#8599,0.980948);
#3428=CIRCLE('',#8600,0.243053047864041);
#3429=CIRCLE('',#8602,0.243053047864041);
#3430=CIRCLE('',#8604,0.980948);
#3431=CIRCLE('',#8605,0.243053047864041);
#3432=CIRCLE('',#8607,0.243053047864041);
#3433=CIRCLE('',#8609,0.980948);
#3434=CIRCLE('',#8610,0.980948);
#3435=CIRCLE('',#8611,0.980948);
#3436=CIRCLE('',#8613,0.243053047864041);
#3437=CIRCLE('',#8615,0.243053047864041);
#3438=CIRCLE('',#8620,1.013815);
#3439=CIRCLE('',#8621,0.991185);
#3440=CIRCLE('',#8623,1.013815);
#3441=CIRCLE('',#8625,0.991185);
#3442=CIRCLE('',#8628,1.013815);
#3443=CIRCLE('',#8629,0.991185);
#3444=CIRCLE('',#8631,1.013815);
#3445=CIRCLE('',#8633,0.991185);
#3446=CIRCLE('',#8650,0.1954);
#3447=CIRCLE('',#8652,0.3);
#3448=CIRCLE('',#8654,0.35);
#3449=CIRCLE('',#8656,0.35);
#3450=CIRCLE('',#8658,0.32);
#3451=CIRCLE('',#8660,0.22);
#3452=CIRCLE('',#8662,0.1954);
#3453=CIRCLE('',#8722,0.164999999999999);
#3454=CIRCLE('',#8723,0.164999999999999);
#3455=CIRCLE('',#8725,0.164999999999999);
#3456=CIRCLE('',#8726,0.164999999999999);
#3457=CIRCLE('',#8728,0.164999999999999);
#3458=CIRCLE('',#8729,0.164999999999999);
#3459=CIRCLE('',#8731,0.504999999999999);
#3460=CIRCLE('',#8732,0.504999999999999);
#3461=CIRCLE('',#8734,0.164999999999999);
#3462=CIRCLE('',#8735,0.164999999999999);
#3463=CIRCLE('',#8737,0.164999999999999);
#3464=CIRCLE('',#8738,0.164999999999999);
#3465=CIRCLE('',#8740,0.164999999999999);
#3466=CIRCLE('',#8741,0.164999999999999);
#3467=CIRCLE('',#8743,0.504999999999999);
#3468=CIRCLE('',#8744,0.504999999999999);
#3469=CIRCLE('',#8746,0.329999999999998);
#3470=CIRCLE('',#8747,0.329999999999998);
#3471=CIRCLE('',#8749,0.329999999999998);
#3472=CIRCLE('',#8750,0.329999999999998);
#3473=CIRCLE('',#8752,0.329999999999998);
#3474=CIRCLE('',#8753,0.329999999999998);
#3475=CIRCLE('',#8755,0.329999999999998);
#3476=CIRCLE('',#8756,0.329999999999998);
#3477=CIRCLE('',#8768,0.164999999999999);
#3478=CIRCLE('',#8769,0.164999999999999);
#3479=CIRCLE('',#8772,0.225000000000001);
#3480=CIRCLE('',#8773,0.225000000000001);
#3481=CIRCLE('',#8775,0.225000000000001);
#3482=CIRCLE('',#8776,0.225000000000001);
#3483=CIRCLE('',#8778,0.225000000000001);
#3484=CIRCLE('',#8779,0.225000000000001);
#3485=CIRCLE('',#8781,1.5);
#3486=CIRCLE('',#8782,0.5);
#3487=CIRCLE('',#8784,1.5);
#3488=CIRCLE('',#8785,0.5);
#3489=CIRCLE('',#8788,0.5);
#3490=CIRCLE('',#8790,0.5);
#3491=CIRCLE('',#8795,0.504999999999999);
#3492=CIRCLE('',#8796,0.504999999999999);
#3493=CIRCLE('',#8798,0.699999999999999);
#3494=CIRCLE('',#8799,0.699999999999999);
#3495=CIRCLE('',#8804,0.504999999999999);
#3496=CIRCLE('',#8805,0.504999999999999);
#3497=CIRCLE('',#8807,0.699999999999999);
#3498=CIRCLE('',#8808,0.699999999999999);
#3499=CIRCLE('',#8813,0.504999999999999);
#3500=CIRCLE('',#8814,0.504999999999999);
#3501=CIRCLE('',#8816,0.699999999999999);
#3502=CIRCLE('',#8817,0.699999999999999);
#3503=CIRCLE('',#8822,0.225000000000001);
#3504=CIRCLE('',#8823,0.225000000000001);
#3505=CIRCLE('',#8825,0.899999999999999);
#3506=CIRCLE('',#8826,0.899999999999999);
#3507=CIRCLE('',#8831,0.164999999999999);
#3508=CIRCLE('',#8832,0.164999999999999);
#3509=CIRCLE('',#8835,0.225000000000001);
#3510=CIRCLE('',#8836,0.225000000000001);
#3511=CIRCLE('',#8838,0.225000000000001);
#3512=CIRCLE('',#8839,0.225000000000001);
#3513=CIRCLE('',#8841,0.225000000000001);
#3514=CIRCLE('',#8842,0.225000000000001);
#3515=CIRCLE('',#8844,1.5);
#3516=CIRCLE('',#8845,0.5);
#3517=CIRCLE('',#8847,1.5);
#3518=CIRCLE('',#8848,0.5);
#3519=CIRCLE('',#8851,0.5);
#3520=CIRCLE('',#8853,0.5);
#3521=CIRCLE('',#8858,0.504999999999999);
#3522=CIRCLE('',#8859,0.504999999999999);
#3523=CIRCLE('',#8861,0.699999999999999);
#3524=CIRCLE('',#8862,0.699999999999999);
#3525=CIRCLE('',#8867,0.504999999999999);
#3526=CIRCLE('',#8868,0.504999999999999);
#3527=CIRCLE('',#8870,0.699999999999999);
#3528=CIRCLE('',#8871,0.699999999999999);
#3529=CIRCLE('',#8876,0.504999999999999);
#3530=CIRCLE('',#8877,0.504999999999999);
#3531=CIRCLE('',#8879,0.699999999999999);
#3532=CIRCLE('',#8880,0.699999999999999);
#3533=CIRCLE('',#8885,0.225000000000001);
#3534=CIRCLE('',#8886,0.225000000000001);
#3535=CIRCLE('',#8888,0.899999999999999);
#3536=CIRCLE('',#8889,0.899999999999999);
#3537=CIRCLE('',#8894,0.3);
#3538=CIRCLE('',#8896,0.35);
#3539=CIRCLE('',#8898,0.35);
#3540=CIRCLE('',#8900,0.32);
#3541=CIRCLE('',#8902,0.22);
#3542=CIRCLE('',#8904,0.1954);
#3543=CIRCLE('',#8906,0.1954);
#3544=CIRCLE('',#8908,0.16);
#3545=VERTEX_POINT('',#11432);
#3546=VERTEX_POINT('',#11434);
#3547=VERTEX_POINT('',#11438);
#3548=VERTEX_POINT('',#11440);
#3549=VERTEX_POINT('',#11444);
#3550=VERTEX_POINT('',#11446);
#3551=VERTEX_POINT('',#11450);
#3552=VERTEX_POINT('',#11452);
#3553=VERTEX_POINT('',#11456);
#3554=VERTEX_POINT('',#11457);
#3555=VERTEX_POINT('',#11459);
#3556=VERTEX_POINT('',#11461);
#3557=VERTEX_POINT('',#11465);
#3558=VERTEX_POINT('',#11467);
#3559=VERTEX_POINT('',#11471);
#3560=VERTEX_POINT('',#11473);
#3561=VERTEX_POINT('',#11483);
#3562=VERTEX_POINT('',#11484);
#3563=VERTEX_POINT('',#11486);
#3564=VERTEX_POINT('',#11488);
#3565=VERTEX_POINT('',#11492);
#3566=VERTEX_POINT('',#11494);
#3567=VERTEX_POINT('',#11498);
#3568=VERTEX_POINT('',#11500);
#3569=VERTEX_POINT('',#11510);
#3570=VERTEX_POINT('',#11511);
#3571=VERTEX_POINT('',#11513);
#3572=VERTEX_POINT('',#11515);
#3573=VERTEX_POINT('',#11519);
#3574=VERTEX_POINT('',#11521);
#3575=VERTEX_POINT('',#11525);
#3576=VERTEX_POINT('',#11527);
#3577=VERTEX_POINT('',#11537);
#3578=VERTEX_POINT('',#11539);
#3579=VERTEX_POINT('',#11544);
#3580=VERTEX_POINT('',#11546);
#3581=VERTEX_POINT('',#11550);
#3582=VERTEX_POINT('',#11552);
#3583=VERTEX_POINT('',#11556);
#3584=VERTEX_POINT('',#11558);
#3585=VERTEX_POINT('',#11562);
#3586=VERTEX_POINT('',#11564);
#3587=VERTEX_POINT('',#11568);
#3588=VERTEX_POINT('',#11570);
#3589=VERTEX_POINT('',#11574);
#3590=VERTEX_POINT('',#11576);
#3591=VERTEX_POINT('',#11580);
#3592=VERTEX_POINT('',#11582);
#3593=VERTEX_POINT('',#11586);
#3594=VERTEX_POINT('',#11588);
#3595=VERTEX_POINT('',#11592);
#3596=VERTEX_POINT('',#11594);
#3597=VERTEX_POINT('',#11598);
#3598=VERTEX_POINT('',#11600);
#3599=VERTEX_POINT('',#11604);
#3600=VERTEX_POINT('',#11606);
#3601=VERTEX_POINT('',#11610);
#3602=VERTEX_POINT('',#11612);
#3603=VERTEX_POINT('',#11616);
#3604=VERTEX_POINT('',#11617);
#3605=VERTEX_POINT('',#11619);
#3606=VERTEX_POINT('',#11621);
#3607=VERTEX_POINT('',#11623);
#3608=VERTEX_POINT('',#11625);
#3609=VERTEX_POINT('',#11627);
#3610=VERTEX_POINT('',#11629);
#3611=VERTEX_POINT('',#11633);
#3612=VERTEX_POINT('',#11635);
#3613=VERTEX_POINT('',#11639);
#3614=VERTEX_POINT('',#11641);
#3615=VERTEX_POINT('',#11649);
#3616=VERTEX_POINT('',#11651);
#3617=VERTEX_POINT('',#11655);
#3618=VERTEX_POINT('',#11659);
#3619=VERTEX_POINT('',#11667);
#3620=VERTEX_POINT('',#11669);
#3621=VERTEX_POINT('',#11674);
#3622=VERTEX_POINT('',#11676);
#3623=VERTEX_POINT('',#11680);
#3624=VERTEX_POINT('',#11682);
#3625=VERTEX_POINT('',#11686);
#3626=VERTEX_POINT('',#11688);
#3627=VERTEX_POINT('',#11692);
#3628=VERTEX_POINT('',#11694);
#3629=VERTEX_POINT('',#11697);
#3630=VERTEX_POINT('',#11699);
#3631=VERTEX_POINT('',#11704);
#3632=VERTEX_POINT('',#11708);
#3633=VERTEX_POINT('',#11715);
#3634=VERTEX_POINT('',#11717);
#3635=VERTEX_POINT('',#11721);
#3636=VERTEX_POINT('',#11723);
#3637=VERTEX_POINT('',#11730);
#3638=VERTEX_POINT('',#11732);
#3639=VERTEX_POINT('',#11736);
#3640=VERTEX_POINT('',#11738);
#3641=VERTEX_POINT('',#11745);
#3642=VERTEX_POINT('',#11747);
#3643=VERTEX_POINT('',#11751);
#3644=VERTEX_POINT('',#11753);
#3645=VERTEX_POINT('',#11760);
#3646=VERTEX_POINT('',#11762);
#3647=VERTEX_POINT('',#11766);
#3648=VERTEX_POINT('',#11768);
#3649=VERTEX_POINT('',#11775);
#3650=VERTEX_POINT('',#11777);
#3651=VERTEX_POINT('',#11782);
#3652=VERTEX_POINT('',#11784);
#3653=VERTEX_POINT('',#11788);
#3654=VERTEX_POINT('',#11790);
#3655=VERTEX_POINT('',#11794);
#3656=VERTEX_POINT('',#11796);
#3657=VERTEX_POINT('',#11800);
#3658=VERTEX_POINT('',#11802);
#3659=VERTEX_POINT('',#11805);
#3660=VERTEX_POINT('',#11807);
#3661=VERTEX_POINT('',#11812);
#3662=VERTEX_POINT('',#11816);
#3663=VERTEX_POINT('',#11823);
#3664=VERTEX_POINT('',#11825);
#3665=VERTEX_POINT('',#11829);
#3666=VERTEX_POINT('',#11831);
#3667=VERTEX_POINT('',#11838);
#3668=VERTEX_POINT('',#11840);
#3669=VERTEX_POINT('',#11844);
#3670=VERTEX_POINT('',#11846);
#3671=VERTEX_POINT('',#11853);
#3672=VERTEX_POINT('',#11855);
#3673=VERTEX_POINT('',#11859);
#3674=VERTEX_POINT('',#11861);
#3675=VERTEX_POINT('',#11868);
#3676=VERTEX_POINT('',#11870);
#3677=VERTEX_POINT('',#11874);
#3678=VERTEX_POINT('',#11876);
#3679=VERTEX_POINT('',#11883);
#3680=VERTEX_POINT('',#11885);
#3681=VERTEX_POINT('',#11889);
#3682=VERTEX_POINT('',#11891);
#3683=VERTEX_POINT('',#11895);
#3684=VERTEX_POINT('',#11896);
#3685=VERTEX_POINT('',#11898);
#3686=VERTEX_POINT('',#11900);
#3687=VERTEX_POINT('',#11904);
#3688=VERTEX_POINT('',#11906);
#3689=VERTEX_POINT('',#11910);
#3690=VERTEX_POINT('',#11912);
#3691=VERTEX_POINT('',#11914);
#3692=VERTEX_POINT('',#11916);
#3693=VERTEX_POINT('',#11918);
#3694=VERTEX_POINT('',#11922);
#3695=VERTEX_POINT('',#11926);
#3696=VERTEX_POINT('',#11927);
#3697=VERTEX_POINT('',#11934);
#3698=VERTEX_POINT('',#11936);
#3699=VERTEX_POINT('',#11940);
#3700=VERTEX_POINT('',#11942);
#3701=VERTEX_POINT('',#11952);
#3702=VERTEX_POINT('',#11954);
#3703=VERTEX_POINT('',#11956);
#3704=VERTEX_POINT('',#11958);
#3705=VERTEX_POINT('',#11975);
#3706=VERTEX_POINT('',#11995);
#3707=VERTEX_POINT('',#11997);
#3708=VERTEX_POINT('',#11999);
#3709=VERTEX_POINT('',#12038);
#3710=VERTEX_POINT('',#12040);
#3711=VERTEX_POINT('',#12591);
#3712=VERTEX_POINT('',#12592);
#3713=VERTEX_POINT('',#12594);
#3714=VERTEX_POINT('',#12596);
#3715=VERTEX_POINT('',#12600);
#3716=VERTEX_POINT('',#12602);
#3717=VERTEX_POINT('',#12606);
#3718=VERTEX_POINT('',#12608);
#3719=VERTEX_POINT('',#12612);
#3720=VERTEX_POINT('',#12614);
#3721=VERTEX_POINT('',#12618);
#3722=VERTEX_POINT('',#12620);
#3723=VERTEX_POINT('',#12629);
#3724=VERTEX_POINT('',#12632);
#3725=VERTEX_POINT('',#12635);
#3726=VERTEX_POINT('',#12639);
#3727=VERTEX_POINT('',#12643);
#3728=VERTEX_POINT('',#12647);
#3729=VERTEX_POINT('',#12650);
#3730=VERTEX_POINT('',#12658);
#3731=VERTEX_POINT('',#12660);
#3732=VERTEX_POINT('',#12664);
#3733=VERTEX_POINT('',#12666);
#3734=VERTEX_POINT('',#12670);
#3735=VERTEX_POINT('',#12672);
#3736=VERTEX_POINT('',#12676);
#3737=VERTEX_POINT('',#12678);
#3738=VERTEX_POINT('',#12682);
#3739=VERTEX_POINT('',#12684);
#3740=VERTEX_POINT('',#12688);
#3741=VERTEX_POINT('',#12690);
#3742=VERTEX_POINT('',#12694);
#3743=VERTEX_POINT('',#12696);
#3744=VERTEX_POINT('',#12700);
#3745=VERTEX_POINT('',#12702);
#3746=VERTEX_POINT('',#12706);
#3747=VERTEX_POINT('',#12708);
#3748=VERTEX_POINT('',#12712);
#3749=VERTEX_POINT('',#12714);
#3750=VERTEX_POINT('',#12718);
#3751=VERTEX_POINT('',#12719);
#3752=VERTEX_POINT('',#12721);
#3753=VERTEX_POINT('',#12723);
#3754=VERTEX_POINT('',#12727);
#3755=VERTEX_POINT('',#12729);
#3756=VERTEX_POINT('',#12733);
#3757=VERTEX_POINT('',#12737);
#3758=VERTEX_POINT('',#12745);
#3759=VERTEX_POINT('',#12747);
#3760=VERTEX_POINT('',#12751);
#3761=VERTEX_POINT('',#12753);
#3762=VERTEX_POINT('',#12760);
#3763=VERTEX_POINT('',#12762);
#3764=VERTEX_POINT('',#12766);
#3765=VERTEX_POINT('',#12768);
#3766=VERTEX_POINT('',#12772);
#3767=VERTEX_POINT('',#12774);
#3768=VERTEX_POINT('',#12778);
#3769=VERTEX_POINT('',#12780);
#3770=VERTEX_POINT('',#12784);
#3771=VERTEX_POINT('',#12786);
#3772=VERTEX_POINT('',#12790);
#3773=VERTEX_POINT('',#12792);
#3774=VERTEX_POINT('',#12799);
#3775=VERTEX_POINT('',#12801);
#3776=VERTEX_POINT('',#12805);
#3777=VERTEX_POINT('',#12807);
#3778=VERTEX_POINT('',#12811);
#3779=VERTEX_POINT('',#12813);
#3780=VERTEX_POINT('',#12817);
#3781=VERTEX_POINT('',#12819);
#3782=VERTEX_POINT('',#12823);
#3783=VERTEX_POINT('',#12825);
#3784=VERTEX_POINT('',#12829);
#3785=VERTEX_POINT('',#12831);
#3786=VERTEX_POINT('',#12838);
#3787=VERTEX_POINT('',#12840);
#3788=VERTEX_POINT('',#12844);
#3789=VERTEX_POINT('',#12846);
#3790=VERTEX_POINT('',#12853);
#3791=VERTEX_POINT('',#12855);
#3792=VERTEX_POINT('',#12859);
#3793=VERTEX_POINT('',#12861);
#3794=VERTEX_POINT('',#12865);
#3795=VERTEX_POINT('',#12867);
#3796=VERTEX_POINT('',#12871);
#3797=VERTEX_POINT('',#12873);
#3798=VERTEX_POINT('',#12877);
#3799=VERTEX_POINT('',#12879);
#3800=VERTEX_POINT('',#12883);
#3801=VERTEX_POINT('',#12885);
#3802=VERTEX_POINT('',#12892);
#3803=VERTEX_POINT('',#12894);
#3804=VERTEX_POINT('',#12898);
#3805=VERTEX_POINT('',#12900);
#3806=VERTEX_POINT('',#12904);
#3807=VERTEX_POINT('',#12906);
#3808=VERTEX_POINT('',#12910);
#3809=VERTEX_POINT('',#12912);
#3810=VERTEX_POINT('',#12916);
#3811=VERTEX_POINT('',#12918);
#3812=VERTEX_POINT('',#12922);
#3813=VERTEX_POINT('',#12924);
#3814=VERTEX_POINT('',#12931);
#3815=VERTEX_POINT('',#12933);
#3816=VERTEX_POINT('',#12937);
#3817=VERTEX_POINT('',#12938);
#3818=VERTEX_POINT('',#12940);
#3819=VERTEX_POINT('',#12942);
#3820=VERTEX_POINT('',#12946);
#3821=VERTEX_POINT('',#12948);
#3822=VERTEX_POINT('',#12952);
#3823=VERTEX_POINT('',#12954);
#3824=VERTEX_POINT('',#12965);
#3825=VERTEX_POINT('',#12967);
#3826=VERTEX_POINT('',#12971);
#3827=VERTEX_POINT('',#12973);
#3828=VERTEX_POINT('',#12977);
#3829=VERTEX_POINT('',#12979);
#3830=VERTEX_POINT('',#12983);
#3831=VERTEX_POINT('',#12985);
#3832=VERTEX_POINT('',#12989);
#3833=VERTEX_POINT('',#12991);
#3834=VERTEX_POINT('',#12995);
#3835=VERTEX_POINT('',#12997);
#3836=VERTEX_POINT('',#13001);
#3837=VERTEX_POINT('',#13003);
#3838=VERTEX_POINT('',#13007);
#3839=VERTEX_POINT('',#13009);
#3840=VERTEX_POINT('',#13013);
#3841=VERTEX_POINT('',#13015);
#3842=VERTEX_POINT('',#13019);
#3843=VERTEX_POINT('',#13021);
#3844=VERTEX_POINT('',#13025);
#3845=VERTEX_POINT('',#13026);
#3846=VERTEX_POINT('',#13028);
#3847=VERTEX_POINT('',#13030);
#3848=VERTEX_POINT('',#13034);
#3849=VERTEX_POINT('',#13036);
#3850=VERTEX_POINT('',#13040);
#3851=VERTEX_POINT('',#13044);
#3852=VERTEX_POINT('',#13052);
#3853=VERTEX_POINT('',#13054);
#3854=VERTEX_POINT('',#13058);
#3855=VERTEX_POINT('',#13060);
#3856=VERTEX_POINT('',#13067);
#3857=VERTEX_POINT('',#13069);
#3858=VERTEX_POINT('',#13073);
#3859=VERTEX_POINT('',#13075);
#3860=VERTEX_POINT('',#13079);
#3861=VERTEX_POINT('',#13081);
#3862=VERTEX_POINT('',#13085);
#3863=VERTEX_POINT('',#13087);
#3864=VERTEX_POINT('',#13091);
#3865=VERTEX_POINT('',#13093);
#3866=VERTEX_POINT('',#13097);
#3867=VERTEX_POINT('',#13099);
#3868=VERTEX_POINT('',#13106);
#3869=VERTEX_POINT('',#13108);
#3870=VERTEX_POINT('',#13112);
#3871=VERTEX_POINT('',#13114);
#3872=VERTEX_POINT('',#13118);
#3873=VERTEX_POINT('',#13120);
#3874=VERTEX_POINT('',#13124);
#3875=VERTEX_POINT('',#13126);
#3876=VERTEX_POINT('',#13130);
#3877=VERTEX_POINT('',#13132);
#3878=VERTEX_POINT('',#13136);
#3879=VERTEX_POINT('',#13138);
#3880=VERTEX_POINT('',#13145);
#3881=VERTEX_POINT('',#13147);
#3882=VERTEX_POINT('',#13151);
#3883=VERTEX_POINT('',#13153);
#3884=VERTEX_POINT('',#13160);
#3885=VERTEX_POINT('',#13162);
#3886=VERTEX_POINT('',#13166);
#3887=VERTEX_POINT('',#13168);
#3888=VERTEX_POINT('',#13172);
#3889=VERTEX_POINT('',#13174);
#3890=VERTEX_POINT('',#13178);
#3891=VERTEX_POINT('',#13180);
#3892=VERTEX_POINT('',#13184);
#3893=VERTEX_POINT('',#13186);
#3894=VERTEX_POINT('',#13190);
#3895=VERTEX_POINT('',#13192);
#3896=VERTEX_POINT('',#13199);
#3897=VERTEX_POINT('',#13201);
#3898=VERTEX_POINT('',#13205);
#3899=VERTEX_POINT('',#13207);
#3900=VERTEX_POINT('',#13211);
#3901=VERTEX_POINT('',#13213);
#3902=VERTEX_POINT('',#13217);
#3903=VERTEX_POINT('',#13219);
#3904=VERTEX_POINT('',#13223);
#3905=VERTEX_POINT('',#13225);
#3906=VERTEX_POINT('',#13229);
#3907=VERTEX_POINT('',#13231);
#3908=VERTEX_POINT('',#13239);
#3909=VERTEX_POINT('',#13240);
#3910=VERTEX_POINT('',#13243);
#3911=VERTEX_POINT('',#13245);
#3912=VERTEX_POINT('',#13249);
#3913=VERTEX_POINT('',#13253);
#3914=VERTEX_POINT('',#13255);
#3915=VERTEX_POINT('',#13259);
#3916=VERTEX_POINT('',#13264);
#3917=VERTEX_POINT('',#13268);
#3918=VERTEX_POINT('',#13274);
#3919=VERTEX_POINT('',#13275);
#3920=VERTEX_POINT('',#13278);
#3921=VERTEX_POINT('',#13280);
#3922=VERTEX_POINT('',#13284);
#3923=VERTEX_POINT('',#13288);
#3924=VERTEX_POINT('',#13290);
#3925=VERTEX_POINT('',#13293);
#3926=VERTEX_POINT('',#13297);
#3927=VERTEX_POINT('',#13301);
#3928=VERTEX_POINT('',#13309);
#3929=VERTEX_POINT('',#13310);
#3930=VERTEX_POINT('',#13313);
#3931=VERTEX_POINT('',#13314);
#3932=VERTEX_POINT('',#13317);
#3933=VERTEX_POINT('',#13318);
#3934=VERTEX_POINT('',#13321);
#3935=VERTEX_POINT('',#13322);
#3936=VERTEX_POINT('',#13325);
#3937=VERTEX_POINT('',#13326);
#3938=VERTEX_POINT('',#13329);
#3939=VERTEX_POINT('',#13330);
#3940=VERTEX_POINT('',#13333);
#3941=VERTEX_POINT('',#13334);
#3942=VERTEX_POINT('',#13337);
#3943=VERTEX_POINT('',#13338);
#3944=VERTEX_POINT('',#13342);
#3945=VERTEX_POINT('',#13343);
#3946=VERTEX_POINT('',#13366);
#3947=VERTEX_POINT('',#13368);
#3948=VERTEX_POINT('',#13393);
#3949=VERTEX_POINT('',#13395);
#3950=VERTEX_POINT('',#13418);
#3951=VERTEX_POINT('',#13420);
#3952=VERTEX_POINT('',#13443);
#3953=VERTEX_POINT('',#13445);
#3954=VERTEX_POINT('',#13458);
#3955=VERTEX_POINT('',#13461);
#3956=VERTEX_POINT('',#13474);
#3957=VERTEX_POINT('',#13476);
#3958=VERTEX_POINT('',#13499);
#3959=VERTEX_POINT('',#13501);
#3960=VERTEX_POINT('',#13524);
#3961=VERTEX_POINT('',#13526);
#3962=VERTEX_POINT('',#13549);
#3963=VERTEX_POINT('',#13551);
#3964=VERTEX_POINT('',#13576);
#3965=VERTEX_POINT('',#13580);
#3966=VERTEX_POINT('',#13605);
#3967=VERTEX_POINT('',#13609);
#3968=VERTEX_POINT('',#13634);
#3969=VERTEX_POINT('',#13638);
#3970=VERTEX_POINT('',#13639);
#3971=VERTEX_POINT('',#13666);
#3972=VERTEX_POINT('',#13670);
#3973=VERTEX_POINT('',#13695);
#3974=VERTEX_POINT('',#13699);
#3975=VERTEX_POINT('',#13724);
#3976=VERTEX_POINT('',#13728);
#3977=VERTEX_POINT('',#13753);
#3978=VERTEX_POINT('',#13756);
#3979=VERTEX_POINT('',#13758);
#3980=VERTEX_POINT('',#13790);
#3981=VERTEX_POINT('',#13792);
#3982=VERTEX_POINT('',#13795);
#3983=VERTEX_POINT('',#13799);
#3984=VERTEX_POINT('',#13804);
#3985=VERTEX_POINT('',#13806);
#3986=VERTEX_POINT('',#13809);
#3987=VERTEX_POINT('',#13813);
#3988=VERTEX_POINT('',#13824);
#3989=VERTEX_POINT('',#13825);
#3990=VERTEX_POINT('',#13827);
#3991=VERTEX_POINT('',#13829);
#3992=VERTEX_POINT('',#13833);
#3993=VERTEX_POINT('',#13835);
#3994=VERTEX_POINT('',#13839);
#3995=VERTEX_POINT('',#13841);
#3996=VERTEX_POINT('',#13845);
#3997=VERTEX_POINT('',#13847);
#3998=VERTEX_POINT('',#13851);
#3999=VERTEX_POINT('',#13853);
#4000=VERTEX_POINT('',#13862);
#4001=VERTEX_POINT('',#13865);
#4002=VERTEX_POINT('',#13868);
#4003=VERTEX_POINT('',#13872);
#4004=VERTEX_POINT('',#13876);
#4005=VERTEX_POINT('',#13880);
#4006=VERTEX_POINT('',#13883);
#4007=VERTEX_POINT('',#13946);
#4008=VERTEX_POINT('',#13948);
#4009=VERTEX_POINT('',#13952);
#4010=VERTEX_POINT('',#13954);
#4011=VERTEX_POINT('',#13958);
#4012=VERTEX_POINT('',#13960);
#4013=VERTEX_POINT('',#13964);
#4014=VERTEX_POINT('',#13966);
#4015=VERTEX_POINT('',#13970);
#4016=VERTEX_POINT('',#13972);
#4017=VERTEX_POINT('',#13976);
#4018=VERTEX_POINT('',#13978);
#4019=VERTEX_POINT('',#13982);
#4020=VERTEX_POINT('',#13984);
#4021=VERTEX_POINT('',#13988);
#4022=VERTEX_POINT('',#13990);
#4023=VERTEX_POINT('',#13994);
#4024=VERTEX_POINT('',#13996);
#4025=VERTEX_POINT('',#14000);
#4026=VERTEX_POINT('',#14002);
#4027=VERTEX_POINT('',#14006);
#4028=VERTEX_POINT('',#14008);
#4029=VERTEX_POINT('',#14012);
#4030=VERTEX_POINT('',#14014);
#4031=VERTEX_POINT('',#14018);
#4032=VERTEX_POINT('',#14019);
#4033=VERTEX_POINT('',#14021);
#4034=VERTEX_POINT('',#14023);
#4035=VERTEX_POINT('',#14027);
#4036=VERTEX_POINT('',#14029);
#4037=VERTEX_POINT('',#14033);
#4038=VERTEX_POINT('',#14037);
#4039=VERTEX_POINT('',#14038);
#4040=VERTEX_POINT('',#14041);
#4041=VERTEX_POINT('',#14045);
#4042=VERTEX_POINT('',#14046);
#4043=VERTEX_POINT('',#14051);
#4044=VERTEX_POINT('',#14055);
#4045=VERTEX_POINT('',#14063);
#4046=VERTEX_POINT('',#14065);
#4047=VERTEX_POINT('',#14070);
#4048=VERTEX_POINT('',#14072);
#4049=VERTEX_POINT('',#14076);
#4050=VERTEX_POINT('',#14078);
#4051=VERTEX_POINT('',#14082);
#4052=VERTEX_POINT('',#14084);
#4053=VERTEX_POINT('',#14088);
#4054=VERTEX_POINT('',#14090);
#4055=VERTEX_POINT('',#14093);
#4056=VERTEX_POINT('',#14095);
#4057=VERTEX_POINT('',#14100);
#4058=VERTEX_POINT('',#14104);
#4059=VERTEX_POINT('',#14111);
#4060=VERTEX_POINT('',#14113);
#4061=VERTEX_POINT('',#14117);
#4062=VERTEX_POINT('',#14119);
#4063=VERTEX_POINT('',#14126);
#4064=VERTEX_POINT('',#14128);
#4065=VERTEX_POINT('',#14132);
#4066=VERTEX_POINT('',#14134);
#4067=VERTEX_POINT('',#14141);
#4068=VERTEX_POINT('',#14143);
#4069=VERTEX_POINT('',#14147);
#4070=VERTEX_POINT('',#14149);
#4071=VERTEX_POINT('',#14156);
#4072=VERTEX_POINT('',#14158);
#4073=VERTEX_POINT('',#14162);
#4074=VERTEX_POINT('',#14164);
#4075=VERTEX_POINT('',#14171);
#4076=VERTEX_POINT('',#14173);
#4077=VERTEX_POINT('',#14178);
#4078=VERTEX_POINT('',#14180);
#4079=VERTEX_POINT('',#14184);
#4080=VERTEX_POINT('',#14186);
#4081=VERTEX_POINT('',#14190);
#4082=VERTEX_POINT('',#14192);
#4083=VERTEX_POINT('',#14196);
#4084=VERTEX_POINT('',#14198);
#4085=VERTEX_POINT('',#14201);
#4086=VERTEX_POINT('',#14203);
#4087=VERTEX_POINT('',#14208);
#4088=VERTEX_POINT('',#14212);
#4089=VERTEX_POINT('',#14219);
#4090=VERTEX_POINT('',#14221);
#4091=VERTEX_POINT('',#14225);
#4092=VERTEX_POINT('',#14227);
#4093=VERTEX_POINT('',#14234);
#4094=VERTEX_POINT('',#14236);
#4095=VERTEX_POINT('',#14240);
#4096=VERTEX_POINT('',#14242);
#4097=VERTEX_POINT('',#14249);
#4098=VERTEX_POINT('',#14251);
#4099=VERTEX_POINT('',#14255);
#4100=VERTEX_POINT('',#14257);
#4101=VERTEX_POINT('',#14264);
#4102=VERTEX_POINT('',#14266);
#4103=VERTEX_POINT('',#14270);
#4104=VERTEX_POINT('',#14272);
#4105=VERTEX_POINT('',#14279);
#4106=VERTEX_POINT('',#14282);
#4107=VERTEX_POINT('',#14286);
#4108=VERTEX_POINT('',#14290);
#4109=VERTEX_POINT('',#14294);
#4110=VERTEX_POINT('',#14297);
#4111=VERTEX_POINT('',#14301);
#4112=VERTEX_POINT('',#14305);
#4113=VERTEX_POINT('',#14310);
#4114=VERTEX_POINT('',#14311);
#4115=VERTEX_POINT('',#14313);
#4116=VERTEX_POINT('',#14315);
#4117=VERTEX_POINT('',#14319);
#4118=VERTEX_POINT('',#14321);
#4119=VERTEX_POINT('',#14325);
#4120=VERTEX_POINT('',#14327);
#4121=VERTEX_POINT('',#14331);
#4122=VERTEX_POINT('',#14333);
#4123=VERTEX_POINT('',#14337);
#4124=VERTEX_POINT('',#14339);
#4125=EDGE_CURVE('',#3545,#3545,#3100,.T.);
#4126=EDGE_CURVE('',#3545,#3546,#2312,.T.);
#4127=EDGE_CURVE('',#3546,#3546,#3101,.T.);
#4128=EDGE_CURVE('',#3547,#3547,#3102,.T.);
#4129=EDGE_CURVE('',#3547,#3548,#2313,.T.);
#4130=EDGE_CURVE('',#3548,#3548,#3103,.T.);
#4131=EDGE_CURVE('',#3549,#3549,#3104,.T.);
#4132=EDGE_CURVE('',#3549,#3550,#2314,.T.);
#4133=EDGE_CURVE('',#3550,#3550,#3105,.T.);
#4134=EDGE_CURVE('',#3551,#3551,#3106,.T.);
#4135=EDGE_CURVE('',#3551,#3552,#2315,.T.);
#4136=EDGE_CURVE('',#3552,#3552,#3107,.T.);
#4137=EDGE_CURVE('',#3553,#3554,#2316,.T.);
#4138=EDGE_CURVE('',#3554,#3555,#2317,.T.);
#4139=EDGE_CURVE('',#3556,#3555,#2318,.T.);
#4140=EDGE_CURVE('',#3553,#3556,#2319,.T.);
#4141=EDGE_CURVE('',#3557,#3553,#2320,.T.);
#4142=EDGE_CURVE('',#3558,#3556,#2321,.T.);
#4143=EDGE_CURVE('',#3557,#3558,#2322,.T.);
#4144=EDGE_CURVE('',#3559,#3557,#2323,.T.);
#4145=EDGE_CURVE('',#3560,#3558,#2324,.T.);
#4146=EDGE_CURVE('',#3559,#3560,#2325,.T.);
#4147=EDGE_CURVE('',#3554,#3559,#2326,.T.);
#4148=EDGE_CURVE('',#3555,#3560,#2327,.T.);
#4149=EDGE_CURVE('',#3561,#3562,#2328,.T.);
#4150=EDGE_CURVE('',#3562,#3563,#2329,.T.);
#4151=EDGE_CURVE('',#3564,#3563,#2330,.T.);
#4152=EDGE_CURVE('',#3561,#3564,#2331,.T.);
#4153=EDGE_CURVE('',#3565,#3561,#2332,.T.);
#4154=EDGE_CURVE('',#3566,#3564,#2333,.T.);
#4155=EDGE_CURVE('',#3565,#3566,#2334,.T.);
#4156=EDGE_CURVE('',#3567,#3565,#2335,.T.);
#4157=EDGE_CURVE('',#3568,#3566,#2336,.T.);
#4158=EDGE_CURVE('',#3567,#3568,#2337,.T.);
#4159=EDGE_CURVE('',#3562,#3567,#2338,.T.);
#4160=EDGE_CURVE('',#3563,#3568,#2339,.T.);
#4161=EDGE_CURVE('',#3569,#3570,#2340,.T.);
#4162=EDGE_CURVE('',#3570,#3571,#2341,.T.);
#4163=EDGE_CURVE('',#3572,#3571,#2342,.T.);
#4164=EDGE_CURVE('',#3569,#3572,#2343,.T.);
#4165=EDGE_CURVE('',#3573,#3569,#2344,.T.);
#4166=EDGE_CURVE('',#3574,#3572,#2345,.T.);
#4167=EDGE_CURVE('',#3573,#3574,#2346,.T.);
#4168=EDGE_CURVE('',#3575,#3573,#2347,.T.);
#4169=EDGE_CURVE('',#3576,#3574,#2348,.T.);
#4170=EDGE_CURVE('',#3575,#3576,#2349,.T.);
#4171=EDGE_CURVE('',#3570,#3575,#2350,.T.);
#4172=EDGE_CURVE('',#3571,#3576,#2351,.T.);
#4173=EDGE_CURVE('',#3577,#3577,#3108,.T.);
#4174=EDGE_CURVE('',#3577,#3578,#2352,.T.);
#4175=EDGE_CURVE('',#3578,#3578,#3109,.T.);
#4176=EDGE_CURVE('',#3579,#3579,#3110,.T.);
#4177=EDGE_CURVE('',#3579,#3580,#2353,.T.);
#4178=EDGE_CURVE('',#3580,#3580,#3111,.T.);
#4179=EDGE_CURVE('',#3581,#3581,#3112,.T.);
#4180=EDGE_CURVE('',#3581,#3582,#2354,.T.);
#4181=EDGE_CURVE('',#3582,#3582,#3113,.T.);
#4182=EDGE_CURVE('',#3583,#3583,#3114,.T.);
#4183=EDGE_CURVE('',#3583,#3584,#2355,.T.);
#4184=EDGE_CURVE('',#3584,#3584,#3115,.T.);
#4185=EDGE_CURVE('',#3585,#3585,#3116,.T.);
#4186=EDGE_CURVE('',#3585,#3586,#2356,.T.);
#4187=EDGE_CURVE('',#3586,#3586,#3117,.T.);
#4188=EDGE_CURVE('',#3587,#3587,#3118,.T.);
#4189=EDGE_CURVE('',#3587,#3588,#2357,.T.);
#4190=EDGE_CURVE('',#3588,#3588,#3119,.T.);
#4191=EDGE_CURVE('',#3589,#3589,#3120,.T.);
#4192=EDGE_CURVE('',#3589,#3590,#2358,.T.);
#4193=EDGE_CURVE('',#3590,#3590,#3121,.T.);
#4194=EDGE_CURVE('',#3591,#3591,#3122,.T.);
#4195=EDGE_CURVE('',#3591,#3592,#2359,.T.);
#4196=EDGE_CURVE('',#3592,#3592,#3123,.T.);
#4197=EDGE_CURVE('',#3593,#3593,#3124,.T.);
#4198=EDGE_CURVE('',#3593,#3594,#2360,.T.);
#4199=EDGE_CURVE('',#3594,#3594,#3125,.T.);
#4200=EDGE_CURVE('',#3595,#3595,#3126,.T.);
#4201=EDGE_CURVE('',#3595,#3596,#2361,.T.);
#4202=EDGE_CURVE('',#3596,#3596,#3127,.T.);
#4203=EDGE_CURVE('',#3597,#3597,#3128,.T.);
#4204=EDGE_CURVE('',#3597,#3598,#2362,.T.);
#4205=EDGE_CURVE('',#3598,#3598,#3129,.T.);
#4206=EDGE_CURVE('',#3599,#3599,#3130,.T.);
#4207=EDGE_CURVE('',#3599,#3600,#2363,.T.);
#4208=EDGE_CURVE('',#3600,#3600,#3131,.T.);
#4209=EDGE_CURVE('',#3601,#3601,#3132,.T.);
#4210=EDGE_CURVE('',#3601,#3602,#2364,.T.);
#4211=EDGE_CURVE('',#3602,#3602,#3133,.T.);
#4212=EDGE_CURVE('',#3603,#3604,#2365,.T.);
#4213=EDGE_CURVE('',#3605,#3603,#2366,.T.);
#4214=EDGE_CURVE('',#3606,#3605,#2367,.T.);
#4215=EDGE_CURVE('',#3607,#3606,#2368,.T.);
#4216=EDGE_CURVE('',#3607,#3608,#2369,.T.);
#4217=EDGE_CURVE('',#3609,#3608,#2370,.T.);
#4218=EDGE_CURVE('',#3610,#3609,#2371,.T.);
#4219=EDGE_CURVE('',#3604,#3610,#2372,.T.);
#4220=EDGE_CURVE('',#3610,#3611,#2373,.T.);
#4221=EDGE_CURVE('',#3612,#3609,#2374,.T.);
#4222=EDGE_CURVE('',#3611,#3612,#2375,.T.);
#4223=EDGE_CURVE('',#3611,#3613,#2376,.T.);
#4224=EDGE_CURVE('',#3614,#3612,#2377,.T.);
#4225=EDGE_CURVE('',#3613,#3614,#2378,.T.);
#4226=EDGE_CURVE('',#3613,#3607,#2379,.T.);
#4227=EDGE_CURVE('',#3608,#3614,#2380,.T.);
#4228=EDGE_CURVE('',#3603,#3615,#2381,.T.);
#4229=EDGE_CURVE('',#3616,#3615,#2382,.T.);
#4230=EDGE_CURVE('',#3605,#3616,#2383,.T.);
#4231=EDGE_CURVE('',#3617,#3616,#2384,.T.);
#4232=EDGE_CURVE('',#3606,#3617,#2385,.T.);
#4233=EDGE_CURVE('',#3618,#3617,#2386,.T.);
#4234=EDGE_CURVE('',#3604,#3618,#2387,.T.);
#4235=EDGE_CURVE('',#3615,#3618,#2388,.T.);
#4236=EDGE_CURVE('',#3619,#3619,#3134,.T.);
#4237=EDGE_CURVE('',#3619,#3620,#2389,.T.);
#4238=EDGE_CURVE('',#3620,#3620,#3135,.T.);
#4239=EDGE_CURVE('',#3621,#3621,#3136,.T.);
#4240=EDGE_CURVE('',#3621,#3622,#2390,.T.);
#4241=EDGE_CURVE('',#3622,#3622,#3137,.T.);
#4242=EDGE_CURVE('',#3623,#3623,#3138,.T.);
#4243=EDGE_CURVE('',#3623,#3624,#2391,.T.);
#4244=EDGE_CURVE('',#3624,#3624,#3139,.T.);
#4245=EDGE_CURVE('',#3625,#3625,#3140,.T.);
#4246=EDGE_CURVE('',#3625,#3626,#2392,.T.);
#4247=EDGE_CURVE('',#3626,#3626,#3141,.T.);
#4248=EDGE_CURVE('',#3627,#3627,#3142,.T.);
#4249=EDGE_CURVE('',#3628,#3628,#3143,.T.);
#4250=EDGE_CURVE('',#3629,#3629,#3144,.T.);
#4251=EDGE_CURVE('',#3630,#3630,#3145,.T.);
#4252=EDGE_CURVE('',#3627,#3629,#2393,.T.);
#4253=EDGE_CURVE('',#3630,#3631,#2394,.T.);
#4254=EDGE_CURVE('',#3631,#3631,#3146,.T.);
#4255=EDGE_CURVE('',#3632,#3632,#3147,.T.);
#4256=EDGE_CURVE('',#3632,#3628,#2395,.T.);
#4257=EDGE_CURVE('',#3633,#3633,#3148,.T.);
#4258=EDGE_CURVE('',#3633,#3634,#2396,.T.);
#4259=EDGE_CURVE('',#3634,#3634,#3149,.T.);
#4260=EDGE_CURVE('',#3635,#3635,#3150,.T.);
#4261=EDGE_CURVE('',#3635,#3636,#2397,.T.);
#4262=EDGE_CURVE('',#3636,#3636,#3151,.T.);
#4263=EDGE_CURVE('',#3637,#3637,#3152,.T.);
#4264=EDGE_CURVE('',#3637,#3638,#2398,.T.);
#4265=EDGE_CURVE('',#3638,#3638,#3153,.T.);
#4266=EDGE_CURVE('',#3639,#3639,#3154,.T.);
#4267=EDGE_CURVE('',#3639,#3640,#2399,.T.);
#4268=EDGE_CURVE('',#3640,#3640,#3155,.T.);
#4269=EDGE_CURVE('',#3641,#3641,#3156,.T.);
#4270=EDGE_CURVE('',#3641,#3642,#2400,.T.);
#4271=EDGE_CURVE('',#3642,#3642,#3157,.T.);
#4272=EDGE_CURVE('',#3643,#3643,#3158,.T.);
#4273=EDGE_CURVE('',#3643,#3644,#2401,.T.);
#4274=EDGE_CURVE('',#3644,#3644,#3159,.T.);
#4275=EDGE_CURVE('',#3645,#3645,#3160,.T.);
#4276=EDGE_CURVE('',#3645,#3646,#2402,.T.);
#4277=EDGE_CURVE('',#3646,#3646,#3161,.T.);
#4278=EDGE_CURVE('',#3647,#3647,#3162,.T.);
#4279=EDGE_CURVE('',#3647,#3648,#2403,.T.);
#4280=EDGE_CURVE('',#3648,#3648,#3163,.T.);
#4281=EDGE_CURVE('',#3649,#3649,#3164,.T.);
#4282=EDGE_CURVE('',#3649,#3650,#2404,.T.);
#4283=EDGE_CURVE('',#3650,#3650,#3165,.T.);
#4284=EDGE_CURVE('',#3651,#3651,#3166,.T.);
#4285=EDGE_CURVE('',#3651,#3652,#2405,.T.);
#4286=EDGE_CURVE('',#3652,#3652,#3167,.T.);
#4287=EDGE_CURVE('',#3653,#3653,#3168,.T.);
#4288=EDGE_CURVE('',#3653,#3654,#2406,.T.);
#4289=EDGE_CURVE('',#3654,#3654,#3169,.T.);
#4290=EDGE_CURVE('',#3655,#3655,#3170,.T.);
#4291=EDGE_CURVE('',#3655,#3656,#2407,.T.);
#4292=EDGE_CURVE('',#3656,#3656,#3171,.T.);
#4293=EDGE_CURVE('',#3657,#3657,#3172,.T.);
#4294=EDGE_CURVE('',#3658,#3658,#3173,.T.);
#4295=EDGE_CURVE('',#3659,#3659,#3174,.T.);
#4296=EDGE_CURVE('',#3660,#3660,#3175,.T.);
#4297=EDGE_CURVE('',#3657,#3659,#2408,.T.);
#4298=EDGE_CURVE('',#3660,#3661,#2409,.T.);
#4299=EDGE_CURVE('',#3661,#3661,#3176,.T.);
#4300=EDGE_CURVE('',#3662,#3662,#3177,.T.);
#4301=EDGE_CURVE('',#3662,#3658,#2410,.T.);
#4302=EDGE_CURVE('',#3663,#3663,#3178,.T.);
#4303=EDGE_CURVE('',#3663,#3664,#2411,.T.);
#4304=EDGE_CURVE('',#3664,#3664,#3179,.T.);
#4305=EDGE_CURVE('',#3665,#3665,#3180,.T.);
#4306=EDGE_CURVE('',#3665,#3666,#2412,.T.);
#4307=EDGE_CURVE('',#3666,#3666,#3181,.T.);
#4308=EDGE_CURVE('',#3667,#3667,#3182,.T.);
#4309=EDGE_CURVE('',#3667,#3668,#2413,.T.);
#4310=EDGE_CURVE('',#3668,#3668,#3183,.T.);
#4311=EDGE_CURVE('',#3669,#3669,#3184,.T.);
#4312=EDGE_CURVE('',#3669,#3670,#2414,.T.);
#4313=EDGE_CURVE('',#3670,#3670,#3185,.T.);
#4314=EDGE_CURVE('',#3671,#3671,#3186,.T.);
#4315=EDGE_CURVE('',#3671,#3672,#2415,.T.);
#4316=EDGE_CURVE('',#3672,#3672,#3187,.T.);
#4317=EDGE_CURVE('',#3673,#3673,#3188,.T.);
#4318=EDGE_CURVE('',#3673,#3674,#2416,.T.);
#4319=EDGE_CURVE('',#3674,#3674,#3189,.T.);
#4320=EDGE_CURVE('',#3675,#3675,#3190,.T.);
#4321=EDGE_CURVE('',#3675,#3676,#2417,.T.);
#4322=EDGE_CURVE('',#3676,#3676,#3191,.T.);
#4323=EDGE_CURVE('',#3677,#3677,#3192,.T.);
#4324=EDGE_CURVE('',#3677,#3678,#2418,.T.);
#4325=EDGE_CURVE('',#3678,#3678,#3193,.T.);
#4326=EDGE_CURVE('',#3679,#3679,#3194,.T.);
#4327=EDGE_CURVE('',#3679,#3680,#2419,.T.);
#4328=EDGE_CURVE('',#3680,#3680,#3195,.T.);
#4329=EDGE_CURVE('',#3681,#3681,#3196,.T.);
#4330=EDGE_CURVE('',#3681,#3682,#2420,.T.);
#4331=EDGE_CURVE('',#3682,#3682,#3197,.T.);
#4332=EDGE_CURVE('',#3683,#3684,#2421,.T.);
#4333=EDGE_CURVE('',#3685,#3683,#2422,.T.);
#4334=EDGE_CURVE('',#3685,#3686,#2423,.T.);
#4335=EDGE_CURVE('',#3684,#3686,#2424,.T.);
#4336=EDGE_CURVE('',#3687,#3685,#2425,.T.);
#4337=EDGE_CURVE('',#3687,#3688,#2426,.T.);
#4338=EDGE_CURVE('',#3686,#3688,#2427,.T.);
#4339=EDGE_CURVE('',#3683,#3689,#2428,.T.);
#4340=EDGE_CURVE('',#3689,#3690,#2429,.T.);
#4341=EDGE_CURVE('',#3691,#3690,#2430,.T.);
#4342=EDGE_CURVE('',#3692,#3691,#2431,.T.);
#4343=EDGE_CURVE('',#3692,#3693,#2432,.T.);
#4344=EDGE_CURVE('',#3693,#3687,#2433,.T.);
#4345=EDGE_CURVE('',#3694,#3684,#2434,.T.);
#4346=EDGE_CURVE('',#3689,#3694,#2435,.T.);
#4347=EDGE_CURVE('',#3695,#3696,#2436,.T.);
#4348=EDGE_CURVE('',#3694,#3696,#2437,.T.);
#4349=EDGE_CURVE('',#3688,#3695,#2438,.T.);
#4350=EDGE_CURVE('',#3693,#3695,#2439,.T.);
#4351=EDGE_CURVE('',#3697,#3692,#2440,.T.);
#4352=EDGE_CURVE('',#3698,#3691,#2441,.T.);
#4353=EDGE_CURVE('',#3697,#3698,#2442,.T.);
#4354=EDGE_CURVE('',#3699,#3697,#2443,.T.);
#4355=EDGE_CURVE('',#3700,#3698,#2444,.T.);
#4356=EDGE_CURVE('',#3699,#3700,#2445,.T.);
#4357=EDGE_CURVE('',#3696,#3699,#2446,.T.);
#4358=EDGE_CURVE('',#3690,#3700,#2447,.T.);
#4359=EDGE_CURVE('',#3701,#3701,#3198,.T.);
#4360=EDGE_CURVE('',#3701,#3702,#2448,.T.);
#4361=EDGE_CURVE('',#3702,#3703,#3199,.T.);
#4362=EDGE_CURVE('',#3704,#3703,#498,.T.);
#4363=EDGE_CURVE('',#3705,#3704,#499,.T.);
#4364=EDGE_CURVE('',#3705,#3702,#3200,.T.);
#4365=EDGE_CURVE('',#3703,#3705,#2449,.T.);
#4366=EDGE_CURVE('',#3705,#3703,#3201,.T.);
#4367=EDGE_CURVE('',#3706,#3706,#3202,.T.);
#4368=EDGE_CURVE('',#3706,#3707,#2450,.T.);
#4369=EDGE_CURVE('',#3708,#3707,#500,.T.);
#4370=EDGE_CURVE('',#3708,#3709,#3203,.T.);
#4371=EDGE_CURVE('',#3710,#3709,#501,.T.);
#4372=EDGE_CURVE('',#3707,#3710,#502,.T.);
#4373=EDGE_CURVE('',#3709,#3708,#2451,.T.);
#4374=EDGE_CURVE('',#3709,#3708,#3204,.T.);
#4375=EDGE_CURVE('',#3710,#3704,#503,.T.);
#4376=EDGE_CURVE('',#3711,#3712,#2452,.T.);
#4377=EDGE_CURVE('',#3712,#3713,#2453,.T.);
#4378=EDGE_CURVE('',#3713,#3714,#2454,.T.);
#4379=EDGE_CURVE('',#3711,#3714,#2455,.T.);
#4380=EDGE_CURVE('',#3712,#3715,#2456,.T.);
#4381=EDGE_CURVE('',#3715,#3716,#2457,.T.);
#4382=EDGE_CURVE('',#3716,#3713,#2458,.T.);
#4383=EDGE_CURVE('',#3715,#3717,#2459,.T.);
#4384=EDGE_CURVE('',#3717,#3718,#2460,.T.);
#4385=EDGE_CURVE('',#3718,#3716,#2461,.T.);
#4386=EDGE_CURVE('',#3717,#3719,#2462,.T.);
#4387=EDGE_CURVE('',#3719,#3720,#2463,.T.);
#4388=EDGE_CURVE('',#3720,#3718,#2464,.T.);
#4389=EDGE_CURVE('',#3719,#3721,#2465,.T.);
#4390=EDGE_CURVE('',#3721,#3722,#2466,.T.);
#4391=EDGE_CURVE('',#3722,#3720,#2467,.T.);
#4392=EDGE_CURVE('',#3721,#3711,#2468,.T.);
#4393=EDGE_CURVE('',#3714,#3722,#2469,.T.);
#4394=EDGE_CURVE('',#3723,#3723,#3205,.T.);
#4395=EDGE_CURVE('',#3724,#3724,#3206,.T.);
#4396=EDGE_CURVE('',#3725,#3725,#3207,.T.);
#4397=EDGE_CURVE('',#3725,#3724,#2470,.T.);
#4398=EDGE_CURVE('',#3726,#3726,#3208,.T.);
#4399=EDGE_CURVE('',#3726,#3725,#2471,.T.);
#4400=EDGE_CURVE('',#3727,#3727,#3209,.T.);
#4401=EDGE_CURVE('',#3727,#3726,#2472,.T.);
#4402=EDGE_CURVE('',#3728,#3728,#3210,.T.);
#4403=EDGE_CURVE('',#3729,#3729,#3211,.F.);
#4404=EDGE_CURVE('',#3729,#3728,#2473,.T.);
#4405=EDGE_CURVE('',#3723,#3729,#2474,.T.);
#4406=EDGE_CURVE('',#3730,#3730,#3212,.T.);
#4407=EDGE_CURVE('',#3730,#3731,#2475,.T.);
#4408=EDGE_CURVE('',#3731,#3731,#3213,.T.);
#4409=EDGE_CURVE('',#3732,#3732,#3214,.T.);
#4410=EDGE_CURVE('',#3732,#3733,#2476,.T.);
#4411=EDGE_CURVE('',#3733,#3733,#3215,.T.);
#4412=EDGE_CURVE('',#3734,#3734,#3216,.T.);
#4413=EDGE_CURVE('',#3734,#3735,#2477,.T.);
#4414=EDGE_CURVE('',#3735,#3735,#3217,.T.);
#4415=EDGE_CURVE('',#3736,#3736,#3218,.T.);
#4416=EDGE_CURVE('',#3736,#3737,#2478,.T.);
#4417=EDGE_CURVE('',#3737,#3737,#3219,.T.);
#4418=EDGE_CURVE('',#3738,#3738,#3220,.T.);
#4419=EDGE_CURVE('',#3738,#3739,#2479,.T.);
#4420=EDGE_CURVE('',#3739,#3739,#3221,.T.);
#4421=EDGE_CURVE('',#3740,#3740,#3222,.T.);
#4422=EDGE_CURVE('',#3740,#3741,#2480,.T.);
#4423=EDGE_CURVE('',#3741,#3741,#3223,.T.);
#4424=EDGE_CURVE('',#3742,#3742,#3224,.T.);
#4425=EDGE_CURVE('',#3742,#3743,#2481,.T.);
#4426=EDGE_CURVE('',#3743,#3743,#3225,.T.);
#4427=EDGE_CURVE('',#3744,#3744,#3226,.T.);
#4428=EDGE_CURVE('',#3744,#3745,#2482,.T.);
#4429=EDGE_CURVE('',#3745,#3745,#3227,.T.);
#4430=EDGE_CURVE('',#3746,#3746,#3228,.T.);
#4431=EDGE_CURVE('',#3746,#3747,#2483,.T.);
#4432=EDGE_CURVE('',#3747,#3747,#3229,.T.);
#4433=EDGE_CURVE('',#3748,#3748,#3230,.T.);
#4434=EDGE_CURVE('',#3748,#3749,#2484,.T.);
#4435=EDGE_CURVE('',#3749,#3749,#3231,.T.);
#4436=EDGE_CURVE('',#3750,#3751,#2485,.T.);
#4437=EDGE_CURVE('',#3752,#3750,#3232,.T.);
#4438=EDGE_CURVE('',#3753,#3752,#2486,.T.);
#4439=EDGE_CURVE('',#3753,#3751,#3233,.T.);
#4440=EDGE_CURVE('',#3754,#3751,#2487,.T.);
#4441=EDGE_CURVE('',#3755,#3754,#2488,.T.);
#4442=EDGE_CURVE('',#3750,#3755,#2489,.T.);
#4443=EDGE_CURVE('',#3753,#3756,#2490,.T.);
#4444=EDGE_CURVE('',#3754,#3756,#3234,.T.);
#4445=EDGE_CURVE('',#3757,#3752,#2491,.T.);
#4446=EDGE_CURVE('',#3756,#3757,#2492,.T.);
#4447=EDGE_CURVE('',#3755,#3757,#3235,.T.);
#4448=EDGE_CURVE('',#3758,#3758,#3236,.T.);
#4449=EDGE_CURVE('',#3758,#3759,#2493,.T.);
#4450=EDGE_CURVE('',#3759,#3759,#3237,.T.);
#4451=EDGE_CURVE('',#3760,#3760,#3238,.T.);
#4452=EDGE_CURVE('',#3760,#3761,#2494,.T.);
#4453=EDGE_CURVE('',#3761,#3761,#3239,.T.);
#4454=EDGE_CURVE('',#3762,#3762,#3240,.T.);
#4455=EDGE_CURVE('',#3762,#3763,#2495,.T.);
#4456=EDGE_CURVE('',#3763,#3763,#3241,.T.);
#4457=EDGE_CURVE('',#3764,#3764,#3242,.T.);
#4458=EDGE_CURVE('',#3764,#3765,#2496,.T.);
#4459=EDGE_CURVE('',#3765,#3765,#3243,.T.);
#4460=EDGE_CURVE('',#3766,#3766,#3244,.T.);
#4461=EDGE_CURVE('',#3766,#3767,#2497,.T.);
#4462=EDGE_CURVE('',#3767,#3767,#3245,.T.);
#4463=EDGE_CURVE('',#3768,#3768,#3246,.T.);
#4464=EDGE_CURVE('',#3768,#3769,#2498,.T.);
#4465=EDGE_CURVE('',#3769,#3769,#3247,.T.);
#4466=EDGE_CURVE('',#3770,#3770,#3248,.T.);
#4467=EDGE_CURVE('',#3770,#3771,#2499,.T.);
#4468=EDGE_CURVE('',#3771,#3771,#3249,.T.);
#4469=EDGE_CURVE('',#3772,#3772,#3250,.T.);
#4470=EDGE_CURVE('',#3772,#3773,#2500,.T.);
#4471=EDGE_CURVE('',#3773,#3773,#3251,.T.);
#4472=EDGE_CURVE('',#3774,#3774,#3252,.T.);
#4473=EDGE_CURVE('',#3774,#3775,#2501,.T.);
#4474=EDGE_CURVE('',#3775,#3775,#3253,.T.);
#4475=EDGE_CURVE('',#3776,#3776,#3254,.T.);
#4476=EDGE_CURVE('',#3776,#3777,#2502,.T.);
#4477=EDGE_CURVE('',#3777,#3777,#3255,.T.);
#4478=EDGE_CURVE('',#3778,#3778,#3256,.T.);
#4479=EDGE_CURVE('',#3778,#3779,#2503,.T.);
#4480=EDGE_CURVE('',#3779,#3779,#3257,.T.);
#4481=EDGE_CURVE('',#3780,#3780,#3258,.T.);
#4482=EDGE_CURVE('',#3780,#3781,#2504,.T.);
#4483=EDGE_CURVE('',#3781,#3781,#3259,.T.);
#4484=EDGE_CURVE('',#3782,#3782,#3260,.T.);
#4485=EDGE_CURVE('',#3782,#3783,#2505,.T.);
#4486=EDGE_CURVE('',#3783,#3783,#3261,.T.);
#4487=EDGE_CURVE('',#3784,#3784,#3262,.T.);
#4488=EDGE_CURVE('',#3784,#3785,#2506,.T.);
#4489=EDGE_CURVE('',#3785,#3785,#3263,.T.);
#4490=EDGE_CURVE('',#3786,#3786,#3264,.T.);
#4491=EDGE_CURVE('',#3786,#3787,#2507,.T.);
#4492=EDGE_CURVE('',#3787,#3787,#3265,.T.);
#4493=EDGE_CURVE('',#3788,#3788,#3266,.T.);
#4494=EDGE_CURVE('',#3788,#3789,#2508,.T.);
#4495=EDGE_CURVE('',#3789,#3789,#3267,.T.);
#4496=EDGE_CURVE('',#3790,#3790,#3268,.T.);
#4497=EDGE_CURVE('',#3790,#3791,#2509,.T.);
#4498=EDGE_CURVE('',#3791,#3791,#3269,.T.);
#4499=EDGE_CURVE('',#3792,#3792,#3270,.T.);
#4500=EDGE_CURVE('',#3792,#3793,#2510,.T.);
#4501=EDGE_CURVE('',#3793,#3793,#3271,.T.);
#4502=EDGE_CURVE('',#3794,#3794,#3272,.T.);
#4503=EDGE_CURVE('',#3794,#3795,#2511,.T.);
#4504=EDGE_CURVE('',#3795,#3795,#3273,.T.);
#4505=EDGE_CURVE('',#3796,#3796,#3274,.T.);
#4506=EDGE_CURVE('',#3796,#3797,#2512,.T.);
#4507=EDGE_CURVE('',#3797,#3797,#3275,.T.);
#4508=EDGE_CURVE('',#3798,#3798,#3276,.T.);
#4509=EDGE_CURVE('',#3798,#3799,#2513,.T.);
#4510=EDGE_CURVE('',#3799,#3799,#3277,.T.);
#4511=EDGE_CURVE('',#3800,#3800,#3278,.T.);
#4512=EDGE_CURVE('',#3800,#3801,#2514,.T.);
#4513=EDGE_CURVE('',#3801,#3801,#3279,.T.);
#4514=EDGE_CURVE('',#3802,#3802,#3280,.T.);
#4515=EDGE_CURVE('',#3802,#3803,#2515,.T.);
#4516=EDGE_CURVE('',#3803,#3803,#3281,.T.);
#4517=EDGE_CURVE('',#3804,#3804,#3282,.T.);
#4518=EDGE_CURVE('',#3804,#3805,#2516,.T.);
#4519=EDGE_CURVE('',#3805,#3805,#3283,.T.);
#4520=EDGE_CURVE('',#3806,#3806,#3284,.T.);
#4521=EDGE_CURVE('',#3806,#3807,#2517,.T.);
#4522=EDGE_CURVE('',#3807,#3807,#3285,.T.);
#4523=EDGE_CURVE('',#3808,#3808,#3286,.T.);
#4524=EDGE_CURVE('',#3808,#3809,#2518,.T.);
#4525=EDGE_CURVE('',#3809,#3809,#3287,.T.);
#4526=EDGE_CURVE('',#3810,#3810,#3288,.T.);
#4527=EDGE_CURVE('',#3810,#3811,#2519,.T.);
#4528=EDGE_CURVE('',#3811,#3811,#3289,.T.);
#4529=EDGE_CURVE('',#3812,#3812,#3290,.T.);
#4530=EDGE_CURVE('',#3812,#3813,#2520,.T.);
#4531=EDGE_CURVE('',#3813,#3813,#3291,.T.);
#4532=EDGE_CURVE('',#3814,#3814,#3292,.T.);
#4533=EDGE_CURVE('',#3814,#3815,#2521,.T.);
#4534=EDGE_CURVE('',#3815,#3815,#3293,.T.);
#4535=EDGE_CURVE('',#3816,#3817,#2522,.T.);
#4536=EDGE_CURVE('',#3817,#3818,#2523,.T.);
#4537=EDGE_CURVE('',#3819,#3818,#2524,.T.);
#4538=EDGE_CURVE('',#3816,#3819,#2525,.T.);
#4539=EDGE_CURVE('',#3820,#3816,#2526,.T.);
#4540=EDGE_CURVE('',#3821,#3819,#2527,.T.);
#4541=EDGE_CURVE('',#3820,#3821,#2528,.T.);
#4542=EDGE_CURVE('',#3822,#3820,#2529,.T.);
#4543=EDGE_CURVE('',#3823,#3821,#2530,.T.);
#4544=EDGE_CURVE('',#3822,#3823,#2531,.T.);
#4545=EDGE_CURVE('',#3817,#3822,#2532,.T.);
#4546=EDGE_CURVE('',#3818,#3823,#2533,.T.);
#4547=EDGE_CURVE('',#3824,#3824,#3294,.T.);
#4548=EDGE_CURVE('',#3824,#3825,#2534,.T.);
#4549=EDGE_CURVE('',#3825,#3825,#3295,.T.);
#4550=EDGE_CURVE('',#3826,#3826,#3296,.T.);
#4551=EDGE_CURVE('',#3826,#3827,#2535,.T.);
#4552=EDGE_CURVE('',#3827,#3827,#3297,.T.);
#4553=EDGE_CURVE('',#3828,#3828,#3298,.T.);
#4554=EDGE_CURVE('',#3828,#3829,#2536,.T.);
#4555=EDGE_CURVE('',#3829,#3829,#3299,.T.);
#4556=EDGE_CURVE('',#3830,#3830,#3300,.T.);
#4557=EDGE_CURVE('',#3830,#3831,#2537,.T.);
#4558=EDGE_CURVE('',#3831,#3831,#3301,.T.);
#4559=EDGE_CURVE('',#3832,#3832,#3302,.T.);
#4560=EDGE_CURVE('',#3832,#3833,#2538,.T.);
#4561=EDGE_CURVE('',#3833,#3833,#3303,.T.);
#4562=EDGE_CURVE('',#3834,#3834,#3304,.T.);
#4563=EDGE_CURVE('',#3834,#3835,#2539,.T.);
#4564=EDGE_CURVE('',#3835,#3835,#3305,.T.);
#4565=EDGE_CURVE('',#3836,#3836,#3306,.T.);
#4566=EDGE_CURVE('',#3836,#3837,#2540,.T.);
#4567=EDGE_CURVE('',#3837,#3837,#3307,.T.);
#4568=EDGE_CURVE('',#3838,#3838,#3308,.T.);
#4569=EDGE_CURVE('',#3838,#3839,#2541,.T.);
#4570=EDGE_CURVE('',#3839,#3839,#3309,.T.);
#4571=EDGE_CURVE('',#3840,#3840,#3310,.T.);
#4572=EDGE_CURVE('',#3840,#3841,#2542,.T.);
#4573=EDGE_CURVE('',#3841,#3841,#3311,.T.);
#4574=EDGE_CURVE('',#3842,#3842,#3312,.T.);
#4575=EDGE_CURVE('',#3842,#3843,#2543,.T.);
#4576=EDGE_CURVE('',#3843,#3843,#3313,.T.);
#4577=EDGE_CURVE('',#3844,#3845,#2544,.T.);
#4578=EDGE_CURVE('',#3846,#3844,#3314,.T.);
#4579=EDGE_CURVE('',#3847,#3846,#2545,.T.);
#4580=EDGE_CURVE('',#3847,#3845,#3315,.T.);
#4581=EDGE_CURVE('',#3848,#3845,#2546,.T.);
#4582=EDGE_CURVE('',#3849,#3848,#2547,.T.);
#4583=EDGE_CURVE('',#3844,#3849,#2548,.T.);
#4584=EDGE_CURVE('',#3847,#3850,#2549,.T.);
#4585=EDGE_CURVE('',#3848,#3850,#3316,.T.);
#4586=EDGE_CURVE('',#3851,#3846,#2550,.T.);
#4587=EDGE_CURVE('',#3850,#3851,#2551,.T.);
#4588=EDGE_CURVE('',#3849,#3851,#3317,.T.);
#4589=EDGE_CURVE('',#3852,#3852,#3318,.T.);
#4590=EDGE_CURVE('',#3852,#3853,#2552,.T.);
#4591=EDGE_CURVE('',#3853,#3853,#3319,.T.);
#4592=EDGE_CURVE('',#3854,#3854,#3320,.T.);
#4593=EDGE_CURVE('',#3854,#3855,#2553,.T.);
#4594=EDGE_CURVE('',#3855,#3855,#3321,.T.);
#4595=EDGE_CURVE('',#3856,#3856,#3322,.T.);
#4596=EDGE_CURVE('',#3856,#3857,#2554,.T.);
#4597=EDGE_CURVE('',#3857,#3857,#3323,.T.);
#4598=EDGE_CURVE('',#3858,#3858,#3324,.T.);
#4599=EDGE_CURVE('',#3858,#3859,#2555,.T.);
#4600=EDGE_CURVE('',#3859,#3859,#3325,.T.);
#4601=EDGE_CURVE('',#3860,#3860,#3326,.T.);
#4602=EDGE_CURVE('',#3860,#3861,#2556,.T.);
#4603=EDGE_CURVE('',#3861,#3861,#3327,.T.);
#4604=EDGE_CURVE('',#3862,#3862,#3328,.T.);
#4605=EDGE_CURVE('',#3862,#3863,#2557,.T.);
#4606=EDGE_CURVE('',#3863,#3863,#3329,.T.);
#4607=EDGE_CURVE('',#3864,#3864,#3330,.T.);
#4608=EDGE_CURVE('',#3864,#3865,#2558,.T.);
#4609=EDGE_CURVE('',#3865,#3865,#3331,.T.);
#4610=EDGE_CURVE('',#3866,#3866,#3332,.T.);
#4611=EDGE_CURVE('',#3866,#3867,#2559,.T.);
#4612=EDGE_CURVE('',#3867,#3867,#3333,.T.);
#4613=EDGE_CURVE('',#3868,#3868,#3334,.T.);
#4614=EDGE_CURVE('',#3868,#3869,#2560,.T.);
#4615=EDGE_CURVE('',#3869,#3869,#3335,.T.);
#4616=EDGE_CURVE('',#3870,#3870,#3336,.T.);
#4617=EDGE_CURVE('',#3870,#3871,#2561,.T.);
#4618=EDGE_CURVE('',#3871,#3871,#3337,.T.);
#4619=EDGE_CURVE('',#3872,#3872,#3338,.T.);
#4620=EDGE_CURVE('',#3872,#3873,#2562,.T.);
#4621=EDGE_CURVE('',#3873,#3873,#3339,.T.);
#4622=EDGE_CURVE('',#3874,#3874,#3340,.T.);
#4623=EDGE_CURVE('',#3874,#3875,#2563,.T.);
#4624=EDGE_CURVE('',#3875,#3875,#3341,.T.);
#4625=EDGE_CURVE('',#3876,#3876,#3342,.T.);
#4626=EDGE_CURVE('',#3876,#3877,#2564,.T.);
#4627=EDGE_CURVE('',#3877,#3877,#3343,.T.);
#4628=EDGE_CURVE('',#3878,#3878,#3344,.T.);
#4629=EDGE_CURVE('',#3878,#3879,#2565,.T.);
#4630=EDGE_CURVE('',#3879,#3879,#3345,.T.);
#4631=EDGE_CURVE('',#3880,#3880,#3346,.T.);
#4632=EDGE_CURVE('',#3880,#3881,#2566,.T.);
#4633=EDGE_CURVE('',#3881,#3881,#3347,.T.);
#4634=EDGE_CURVE('',#3882,#3882,#3348,.T.);
#4635=EDGE_CURVE('',#3882,#3883,#2567,.T.);
#4636=EDGE_CURVE('',#3883,#3883,#3349,.T.);
#4637=EDGE_CURVE('',#3884,#3884,#3350,.T.);
#4638=EDGE_CURVE('',#3884,#3885,#2568,.T.);
#4639=EDGE_CURVE('',#3885,#3885,#3351,.T.);
#4640=EDGE_CURVE('',#3886,#3886,#3352,.T.);
#4641=EDGE_CURVE('',#3886,#3887,#2569,.T.);
#4642=EDGE_CURVE('',#3887,#3887,#3353,.T.);
#4643=EDGE_CURVE('',#3888,#3888,#3354,.T.);
#4644=EDGE_CURVE('',#3888,#3889,#2570,.T.);
#4645=EDGE_CURVE('',#3889,#3889,#3355,.T.);
#4646=EDGE_CURVE('',#3890,#3890,#3356,.T.);
#4647=EDGE_CURVE('',#3890,#3891,#2571,.T.);
#4648=EDGE_CURVE('',#3891,#3891,#3357,.T.);
#4649=EDGE_CURVE('',#3892,#3892,#3358,.T.);
#4650=EDGE_CURVE('',#3892,#3893,#2572,.T.);
#4651=EDGE_CURVE('',#3893,#3893,#3359,.T.);
#4652=EDGE_CURVE('',#3894,#3894,#3360,.T.);
#4653=EDGE_CURVE('',#3894,#3895,#2573,.T.);
#4654=EDGE_CURVE('',#3895,#3895,#3361,.T.);
#4655=EDGE_CURVE('',#3896,#3896,#3362,.T.);
#4656=EDGE_CURVE('',#3896,#3897,#2574,.T.);
#4657=EDGE_CURVE('',#3897,#3897,#3363,.T.);
#4658=EDGE_CURVE('',#3898,#3898,#3364,.T.);
#4659=EDGE_CURVE('',#3898,#3899,#2575,.T.);
#4660=EDGE_CURVE('',#3899,#3899,#3365,.T.);
#4661=EDGE_CURVE('',#3900,#3900,#3366,.T.);
#4662=EDGE_CURVE('',#3900,#3901,#2576,.T.);
#4663=EDGE_CURVE('',#3901,#3901,#3367,.T.);
#4664=EDGE_CURVE('',#3902,#3902,#3368,.T.);
#4665=EDGE_CURVE('',#3902,#3903,#2577,.T.);
#4666=EDGE_CURVE('',#3903,#3903,#3369,.T.);
#4667=EDGE_CURVE('',#3904,#3904,#3370,.T.);
#4668=EDGE_CURVE('',#3904,#3905,#2578,.T.);
#4669=EDGE_CURVE('',#3905,#3905,#3371,.T.);
#4670=EDGE_CURVE('',#3906,#3906,#3372,.T.);
#4671=EDGE_CURVE('',#3906,#3907,#2579,.T.);
#4672=EDGE_CURVE('',#3907,#3907,#3373,.T.);
#4673=EDGE_CURVE('',#3908,#3909,#3374,.T.);
#4674=EDGE_CURVE('',#3909,#3908,#3375,.T.);
#4675=EDGE_CURVE('',#3909,#3910,#3376,.T.);
#4676=EDGE_CURVE('',#3911,#3910,#3377,.T.);
#4677=EDGE_CURVE('',#3910,#3911,#3378,.T.);
#4678=EDGE_CURVE('',#3911,#3912,#2580,.T.);
#4679=EDGE_CURVE('',#3912,#3912,#3379,.T.);
#4680=EDGE_CURVE('',#3913,#3913,#3380,.T.);
#4681=EDGE_CURVE('',#3913,#3914,#2581,.T.);
#4682=EDGE_CURVE('',#3914,#3914,#3381,.T.);
#4683=EDGE_CURVE('',#3914,#3915,#2582,.T.);
#4684=EDGE_CURVE('',#3915,#3915,#3382,.T.);
#4685=EDGE_CURVE('',#3916,#3916,#3383,.T.);
#4686=EDGE_CURVE('',#3916,#3908,#2583,.T.);
#4687=EDGE_CURVE('',#3917,#3917,#3384,.T.);
#4688=EDGE_CURVE('',#3917,#3913,#2584,.T.);
#4689=EDGE_CURVE('',#3918,#3919,#3385,.T.);
#4690=EDGE_CURVE('',#3919,#3918,#3386,.T.);
#4691=EDGE_CURVE('',#3919,#3920,#3387,.T.);
#4692=EDGE_CURVE('',#3921,#3920,#3388,.T.);
#4693=EDGE_CURVE('',#3920,#3921,#3389,.T.);
#4694=EDGE_CURVE('',#3922,#3922,#3390,.T.);
#4695=EDGE_CURVE('',#3922,#3921,#2585,.T.);
#4696=EDGE_CURVE('',#3923,#3923,#3391,.T.);
#4697=EDGE_CURVE('',#3924,#3924,#3392,.T.);
#4698=EDGE_CURVE('',#3925,#3925,#3393,.T.);
#4699=EDGE_CURVE('',#3925,#3923,#2586,.T.);
#4700=EDGE_CURVE('',#3926,#3926,#3394,.T.);
#4701=EDGE_CURVE('',#3926,#3925,#2587,.T.);
#4702=EDGE_CURVE('',#3927,#3927,#3395,.T.);
#4703=EDGE_CURVE('',#3927,#3926,#2588,.T.);
#4704=EDGE_CURVE('',#3918,#3924,#2589,.T.);
#4705=EDGE_CURVE('',#3928,#3929,#3396,.T.);
#4706=EDGE_CURVE('',#3930,#3931,#3397,.T.);
#4707=EDGE_CURVE('',#3932,#3933,#3398,.T.);
#4708=EDGE_CURVE('',#3934,#3935,#3399,.T.);
#4709=EDGE_CURVE('',#3936,#3937,#3400,.T.);
#4710=EDGE_CURVE('',#3938,#3939,#3401,.T.);
#4711=EDGE_CURVE('',#3940,#3941,#3402,.T.);
#4712=EDGE_CURVE('',#3942,#3943,#3403,.T.);
#4713=EDGE_CURVE('',#3944,#3945,#504,.T.);
#4714=EDGE_CURVE('',#3946,#3944,#3404,.T.);
#4715=EDGE_CURVE('',#3947,#3946,#505,.T.);
#4716=EDGE_CURVE('',#3945,#3947,#3405,.T.);
#4717=EDGE_CURVE('',#3948,#3946,#3406,.T.);
#4718=EDGE_CURVE('',#3948,#3949,#506,.T.);
#4719=EDGE_CURVE('',#3950,#3949,#3407,.T.);
#4720=EDGE_CURVE('',#3950,#3951,#507,.T.);
#4721=EDGE_CURVE('',#3952,#3951,#3408,.T.);
#4722=EDGE_CURVE('',#3952,#3953,#508,.T.);
#4723=EDGE_CURVE('',#3953,#3954,#2590,.T.);
#4724=EDGE_CURVE('',#3954,#3954,#3409,.T.);
#4725=EDGE_CURVE('',#3953,#3955,#509,.T.);
#4726=EDGE_CURVE('',#3956,#3955,#3410,.T.);
#4727=EDGE_CURVE('',#3956,#3957,#510,.T.);
#4728=EDGE_CURVE('',#3958,#3957,#3411,.T.);
#4729=EDGE_CURVE('',#3958,#3959,#511,.T.);
#4730=EDGE_CURVE('',#3960,#3959,#3412,.T.);
#4731=EDGE_CURVE('',#3960,#3961,#512,.T.);
#4732=EDGE_CURVE('',#3962,#3961,#3413,.T.);
#4733=EDGE_CURVE('',#3962,#3963,#513,.T.);
#4734=EDGE_CURVE('',#3947,#3963,#3414,.T.);
#4735=EDGE_CURVE('',#3944,#3964,#3415,.T.);
#4736=EDGE_CURVE('',#3964,#3948,#3416,.T.);
#4737=EDGE_CURVE('',#3965,#3964,#514,.T.);
#4738=EDGE_CURVE('',#3949,#3965,#3417,.T.);
#4739=EDGE_CURVE('',#3965,#3966,#3418,.T.);
#4740=EDGE_CURVE('',#3966,#3950,#3419,.T.);
#4741=EDGE_CURVE('',#3967,#3966,#515,.T.);
#4742=EDGE_CURVE('',#3951,#3967,#3420,.T.);
#4743=EDGE_CURVE('',#3967,#3968,#3421,.T.);
#4744=EDGE_CURVE('',#3968,#3952,#3422,.T.);
#4745=EDGE_CURVE('',#3969,#3970,#516,.T.);
#4746=EDGE_CURVE('',#3955,#3969,#3423,.T.);
#4747=EDGE_CURVE('',#3970,#3968,#517,.T.);
#4748=EDGE_CURVE('',#3969,#3971,#3424,.T.);
#4749=EDGE_CURVE('',#3971,#3956,#3425,.T.);
#4750=EDGE_CURVE('',#3972,#3971,#518,.T.);
#4751=EDGE_CURVE('',#3957,#3972,#3426,.T.);
#4752=EDGE_CURVE('',#3972,#3973,#3427,.T.);
#4753=EDGE_CURVE('',#3973,#3958,#3428,.T.);
#4754=EDGE_CURVE('',#3974,#3973,#519,.T.);
#4755=EDGE_CURVE('',#3959,#3974,#3429,.T.);
#4756=EDGE_CURVE('',#3974,#3975,#3430,.T.);
#4757=EDGE_CURVE('',#3975,#3960,#3431,.T.);
#4758=EDGE_CURVE('',#3976,#3975,#520,.T.);
#4759=EDGE_CURVE('',#3961,#3976,#3432,.T.);
#4760=EDGE_CURVE('',#3977,#3977,#3433,.T.);
#4761=EDGE_CURVE('',#3977,#3970,#2591,.T.);
#4762=EDGE_CURVE('',#3978,#3945,#3434,.T.);
#4763=EDGE_CURVE('',#3978,#3979,#521,.T.);
#4764=EDGE_CURVE('',#3976,#3979,#3435,.T.);
#4765=EDGE_CURVE('',#3963,#3978,#3436,.T.);
#4766=EDGE_CURVE('',#3979,#3962,#3437,.T.);
#4767=EDGE_CURVE('',#3980,#3980,#3438,.T.);
#4768=EDGE_CURVE('',#3981,#3981,#3439,.T.);
#4769=EDGE_CURVE('',#3982,#3982,#3440,.T.);
#4770=EDGE_CURVE('',#3982,#3980,#2592,.T.);
#4771=EDGE_CURVE('',#3983,#3983,#3441,.T.);
#4772=EDGE_CURVE('',#3983,#3981,#2593,.T.);
#4773=EDGE_CURVE('',#3984,#3984,#3442,.T.);
#4774=EDGE_CURVE('',#3985,#3985,#3443,.T.);
#4775=EDGE_CURVE('',#3986,#3986,#3444,.T.);
#4776=EDGE_CURVE('',#3986,#3984,#2594,.T.);
#4777=EDGE_CURVE('',#3987,#3987,#3445,.T.);
#4778=EDGE_CURVE('',#3987,#3985,#2595,.T.);
#4779=EDGE_CURVE('',#3988,#3989,#2596,.T.);
#4780=EDGE_CURVE('',#3989,#3990,#2597,.T.);
#4781=EDGE_CURVE('',#3990,#3991,#2598,.T.);
#4782=EDGE_CURVE('',#3988,#3991,#2599,.T.);
#4783=EDGE_CURVE('',#3989,#3992,#2600,.T.);
#4784=EDGE_CURVE('',#3992,#3993,#2601,.T.);
#4785=EDGE_CURVE('',#3993,#3990,#2602,.T.);
#4786=EDGE_CURVE('',#3992,#3994,#2603,.T.);
#4787=EDGE_CURVE('',#3994,#3995,#2604,.T.);
#4788=EDGE_CURVE('',#3995,#3993,#2605,.T.);
#4789=EDGE_CURVE('',#3994,#3996,#2606,.T.);
#4790=EDGE_CURVE('',#3996,#3997,#2607,.T.);
#4791=EDGE_CURVE('',#3997,#3995,#2608,.T.);
#4792=EDGE_CURVE('',#3996,#3998,#2609,.T.);
#4793=EDGE_CURVE('',#3998,#3999,#2610,.T.);
#4794=EDGE_CURVE('',#3999,#3997,#2611,.T.);
#4795=EDGE_CURVE('',#3998,#3988,#2612,.T.);
#4796=EDGE_CURVE('',#3991,#3999,#2613,.T.);
#4797=EDGE_CURVE('',#4000,#4000,#3446,.T.);
#4798=EDGE_CURVE('',#4001,#4001,#3447,.T.);
#4799=EDGE_CURVE('',#4002,#4002,#3448,.T.);
#4800=EDGE_CURVE('',#4002,#4001,#2614,.T.);
#4801=EDGE_CURVE('',#4003,#4003,#3449,.T.);
#4802=EDGE_CURVE('',#4003,#4002,#2615,.T.);
#4803=EDGE_CURVE('',#4004,#4004,#3450,.T.);
#4804=EDGE_CURVE('',#4004,#4003,#2616,.T.);
#4805=EDGE_CURVE('',#4005,#4005,#3451,.T.);
#4806=EDGE_CURVE('',#4006,#4006,#3452,.F.);
#4807=EDGE_CURVE('',#4006,#4005,#2617,.T.);
#4808=EDGE_CURVE('',#4000,#4006,#2618,.T.);
#4809=EDGE_CURVE('',#4007,#4007,#3453,.T.);
#4810=EDGE_CURVE('',#4007,#4008,#2619,.T.);
#4811=EDGE_CURVE('',#4008,#4008,#3454,.T.);
#4812=EDGE_CURVE('',#4009,#4009,#3455,.T.);
#4813=EDGE_CURVE('',#4009,#4010,#2620,.T.);
#4814=EDGE_CURVE('',#4010,#4010,#3456,.T.);
#4815=EDGE_CURVE('',#4011,#4011,#3457,.T.);
#4816=EDGE_CURVE('',#4011,#4012,#2621,.T.);
#4817=EDGE_CURVE('',#4012,#4012,#3458,.T.);
#4818=EDGE_CURVE('',#4013,#4013,#3459,.T.);
#4819=EDGE_CURVE('',#4013,#4014,#2622,.T.);
#4820=EDGE_CURVE('',#4014,#4014,#3460,.T.);
#4821=EDGE_CURVE('',#4015,#4015,#3461,.T.);
#4822=EDGE_CURVE('',#4015,#4016,#2623,.T.);
#4823=EDGE_CURVE('',#4016,#4016,#3462,.T.);
#4824=EDGE_CURVE('',#4017,#4017,#3463,.T.);
#4825=EDGE_CURVE('',#4017,#4018,#2624,.T.);
#4826=EDGE_CURVE('',#4018,#4018,#3464,.T.);
#4827=EDGE_CURVE('',#4019,#4019,#3465,.T.);
#4828=EDGE_CURVE('',#4019,#4020,#2625,.T.);
#4829=EDGE_CURVE('',#4020,#4020,#3466,.T.);
#4830=EDGE_CURVE('',#4021,#4021,#3467,.T.);
#4831=EDGE_CURVE('',#4021,#4022,#2626,.T.);
#4832=EDGE_CURVE('',#4022,#4022,#3468,.T.);
#4833=EDGE_CURVE('',#4023,#4023,#3469,.T.);
#4834=EDGE_CURVE('',#4023,#4024,#2627,.T.);
#4835=EDGE_CURVE('',#4024,#4024,#3470,.T.);
#4836=EDGE_CURVE('',#4025,#4025,#3471,.T.);
#4837=EDGE_CURVE('',#4025,#4026,#2628,.T.);
#4838=EDGE_CURVE('',#4026,#4026,#3472,.T.);
#4839=EDGE_CURVE('',#4027,#4027,#3473,.T.);
#4840=EDGE_CURVE('',#4027,#4028,#2629,.T.);
#4841=EDGE_CURVE('',#4028,#4028,#3474,.T.);
#4842=EDGE_CURVE('',#4029,#4029,#3475,.T.);
#4843=EDGE_CURVE('',#4029,#4030,#2630,.T.);
#4844=EDGE_CURVE('',#4030,#4030,#3476,.T.);
#4845=EDGE_CURVE('',#4031,#4032,#2631,.T.);
#4846=EDGE_CURVE('',#4032,#4033,#2632,.T.);
#4847=EDGE_CURVE('',#4034,#4033,#2633,.T.);
#4848=EDGE_CURVE('',#4031,#4034,#2634,.T.);
#4849=EDGE_CURVE('',#4035,#4031,#2635,.T.);
#4850=EDGE_CURVE('',#4036,#4034,#2636,.T.);
#4851=EDGE_CURVE('',#4035,#4036,#2637,.T.);
#4852=EDGE_CURVE('',#4033,#4037,#2638,.T.);
#4853=EDGE_CURVE('',#4037,#4036,#2639,.T.);
#4854=EDGE_CURVE('',#4038,#4039,#2640,.T.);
#4855=EDGE_CURVE('',#4032,#4039,#2641,.T.);
#4856=EDGE_CURVE('',#4040,#4035,#2642,.T.);
#4857=EDGE_CURVE('',#4040,#4038,#2643,.T.);
#4858=EDGE_CURVE('',#4041,#4042,#2644,.T.);
#4859=EDGE_CURVE('',#4042,#4039,#2645,.T.);
#4860=EDGE_CURVE('',#4041,#4038,#2646,.T.);
#4861=EDGE_CURVE('',#4043,#4041,#2647,.T.);
#4862=EDGE_CURVE('',#4043,#4040,#2648,.T.);
#4863=EDGE_CURVE('',#4044,#4043,#2649,.T.);
#4864=EDGE_CURVE('',#4044,#4037,#2650,.T.);
#4865=EDGE_CURVE('',#4042,#4044,#2651,.T.);
#4866=EDGE_CURVE('',#4045,#4045,#3477,.T.);
#4867=EDGE_CURVE('',#4045,#4046,#2652,.T.);
#4868=EDGE_CURVE('',#4046,#4046,#3478,.T.);
#4869=EDGE_CURVE('',#4047,#4047,#3479,.T.);
#4870=EDGE_CURVE('',#4047,#4048,#2653,.T.);
#4871=EDGE_CURVE('',#4048,#4048,#3480,.T.);
#4872=EDGE_CURVE('',#4049,#4049,#3481,.T.);
#4873=EDGE_CURVE('',#4049,#4050,#2654,.T.);
#4874=EDGE_CURVE('',#4050,#4050,#3482,.T.);
#4875=EDGE_CURVE('',#4051,#4051,#3483,.T.);
#4876=EDGE_CURVE('',#4051,#4052,#2655,.T.);
#4877=EDGE_CURVE('',#4052,#4052,#3484,.T.);
#4878=EDGE_CURVE('',#4053,#4053,#3485,.T.);
#4879=EDGE_CURVE('',#4054,#4054,#3486,.T.);
#4880=EDGE_CURVE('',#4055,#4055,#3487,.T.);
#4881=EDGE_CURVE('',#4056,#4056,#3488,.T.);
#4882=EDGE_CURVE('',#4053,#4055,#2656,.T.);
#4883=EDGE_CURVE('',#4056,#4057,#2657,.T.);
#4884=EDGE_CURVE('',#4057,#4057,#3489,.T.);
#4885=EDGE_CURVE('',#4058,#4058,#3490,.T.);
#4886=EDGE_CURVE('',#4058,#4054,#2658,.T.);
#4887=EDGE_CURVE('',#4059,#4059,#3491,.T.);
#4888=EDGE_CURVE('',#4059,#4060,#2659,.T.);
#4889=EDGE_CURVE('',#4060,#4060,#3492,.T.);
#4890=EDGE_CURVE('',#4061,#4061,#3493,.T.);
#4891=EDGE_CURVE('',#4061,#4062,#2660,.T.);
#4892=EDGE_CURVE('',#4062,#4062,#3494,.T.);
#4893=EDGE_CURVE('',#4063,#4063,#3495,.T.);
#4894=EDGE_CURVE('',#4063,#4064,#2661,.T.);
#4895=EDGE_CURVE('',#4064,#4064,#3496,.T.);
#4896=EDGE_CURVE('',#4065,#4065,#3497,.T.);
#4897=EDGE_CURVE('',#4065,#4066,#2662,.T.);
#4898=EDGE_CURVE('',#4066,#4066,#3498,.T.);
#4899=EDGE_CURVE('',#4067,#4067,#3499,.T.);
#4900=EDGE_CURVE('',#4067,#4068,#2663,.T.);
#4901=EDGE_CURVE('',#4068,#4068,#3500,.T.);
#4902=EDGE_CURVE('',#4069,#4069,#3501,.T.);
#4903=EDGE_CURVE('',#4069,#4070,#2664,.T.);
#4904=EDGE_CURVE('',#4070,#4070,#3502,.T.);
#4905=EDGE_CURVE('',#4071,#4071,#3503,.T.);
#4906=EDGE_CURVE('',#4071,#4072,#2665,.T.);
#4907=EDGE_CURVE('',#4072,#4072,#3504,.T.);
#4908=EDGE_CURVE('',#4073,#4073,#3505,.T.);
#4909=EDGE_CURVE('',#4073,#4074,#2666,.T.);
#4910=EDGE_CURVE('',#4074,#4074,#3506,.T.);
#4911=EDGE_CURVE('',#4075,#4075,#3507,.T.);
#4912=EDGE_CURVE('',#4075,#4076,#2667,.T.);
#4913=EDGE_CURVE('',#4076,#4076,#3508,.T.);
#4914=EDGE_CURVE('',#4077,#4077,#3509,.T.);
#4915=EDGE_CURVE('',#4077,#4078,#2668,.T.);
#4916=EDGE_CURVE('',#4078,#4078,#3510,.T.);
#4917=EDGE_CURVE('',#4079,#4079,#3511,.T.);
#4918=EDGE_CURVE('',#4079,#4080,#2669,.T.);
#4919=EDGE_CURVE('',#4080,#4080,#3512,.T.);
#4920=EDGE_CURVE('',#4081,#4081,#3513,.T.);
#4921=EDGE_CURVE('',#4081,#4082,#2670,.T.);
#4922=EDGE_CURVE('',#4082,#4082,#3514,.T.);
#4923=EDGE_CURVE('',#4083,#4083,#3515,.T.);
#4924=EDGE_CURVE('',#4084,#4084,#3516,.T.);
#4925=EDGE_CURVE('',#4085,#4085,#3517,.T.);
#4926=EDGE_CURVE('',#4086,#4086,#3518,.T.);
#4927=EDGE_CURVE('',#4083,#4085,#2671,.T.);
#4928=EDGE_CURVE('',#4086,#4087,#2672,.T.);
#4929=EDGE_CURVE('',#4087,#4087,#3519,.T.);
#4930=EDGE_CURVE('',#4088,#4088,#3520,.T.);
#4931=EDGE_CURVE('',#4088,#4084,#2673,.T.);
#4932=EDGE_CURVE('',#4089,#4089,#3521,.T.);
#4933=EDGE_CURVE('',#4089,#4090,#2674,.T.);
#4934=EDGE_CURVE('',#4090,#4090,#3522,.T.);
#4935=EDGE_CURVE('',#4091,#4091,#3523,.T.);
#4936=EDGE_CURVE('',#4091,#4092,#2675,.T.);
#4937=EDGE_CURVE('',#4092,#4092,#3524,.T.);
#4938=EDGE_CURVE('',#4093,#4093,#3525,.T.);
#4939=EDGE_CURVE('',#4093,#4094,#2676,.T.);
#4940=EDGE_CURVE('',#4094,#4094,#3526,.T.);
#4941=EDGE_CURVE('',#4095,#4095,#3527,.T.);
#4942=EDGE_CURVE('',#4095,#4096,#2677,.T.);
#4943=EDGE_CURVE('',#4096,#4096,#3528,.T.);
#4944=EDGE_CURVE('',#4097,#4097,#3529,.T.);
#4945=EDGE_CURVE('',#4097,#4098,#2678,.T.);
#4946=EDGE_CURVE('',#4098,#4098,#3530,.T.);
#4947=EDGE_CURVE('',#4099,#4099,#3531,.T.);
#4948=EDGE_CURVE('',#4099,#4100,#2679,.T.);
#4949=EDGE_CURVE('',#4100,#4100,#3532,.T.);
#4950=EDGE_CURVE('',#4101,#4101,#3533,.T.);
#4951=EDGE_CURVE('',#4101,#4102,#2680,.T.);
#4952=EDGE_CURVE('',#4102,#4102,#3534,.T.);
#4953=EDGE_CURVE('',#4103,#4103,#3535,.T.);
#4954=EDGE_CURVE('',#4103,#4104,#2681,.T.);
#4955=EDGE_CURVE('',#4104,#4104,#3536,.T.);
#4956=EDGE_CURVE('',#4105,#4105,#3537,.T.);
#4957=EDGE_CURVE('',#4106,#4106,#3538,.T.);
#4958=EDGE_CURVE('',#4106,#4105,#2682,.T.);
#4959=EDGE_CURVE('',#4107,#4107,#3539,.T.);
#4960=EDGE_CURVE('',#4107,#4106,#2683,.T.);
#4961=EDGE_CURVE('',#4108,#4108,#3540,.T.);
#4962=EDGE_CURVE('',#4108,#4107,#2684,.T.);
#4963=EDGE_CURVE('',#4109,#4109,#3541,.T.);
#4964=EDGE_CURVE('',#4110,#4110,#3542,.F.);
#4965=EDGE_CURVE('',#4110,#4109,#2685,.T.);
#4966=EDGE_CURVE('',#4111,#4111,#3543,.F.);
#4967=EDGE_CURVE('',#4111,#4110,#2686,.T.);
#4968=EDGE_CURVE('',#4112,#4112,#3544,.T.);
#4969=EDGE_CURVE('',#4112,#4111,#2687,.T.);
#4970=EDGE_CURVE('',#4113,#4114,#2688,.T.);
#4971=EDGE_CURVE('',#4114,#4115,#2689,.T.);
#4972=EDGE_CURVE('',#4115,#4116,#2690,.T.);
#4973=EDGE_CURVE('',#4113,#4116,#2691,.T.);
#4974=EDGE_CURVE('',#4114,#4117,#2692,.T.);
#4975=EDGE_CURVE('',#4117,#4118,#2693,.T.);
#4976=EDGE_CURVE('',#4118,#4115,#2694,.T.);
#4977=EDGE_CURVE('',#4117,#4119,#2695,.T.);
#4978=EDGE_CURVE('',#4119,#4120,#2696,.T.);
#4979=EDGE_CURVE('',#4120,#4118,#2697,.T.);
#4980=EDGE_CURVE('',#4119,#4121,#2698,.T.);
#4981=EDGE_CURVE('',#4121,#4122,#2699,.T.);
#4982=EDGE_CURVE('',#4122,#4120,#2700,.T.);
#4983=EDGE_CURVE('',#4121,#4123,#2701,.T.);
#4984=EDGE_CURVE('',#4123,#4124,#2702,.T.);
#4985=EDGE_CURVE('',#4124,#4122,#2703,.T.);
#4986=EDGE_CURVE('',#4123,#4113,#2704,.T.);
#4987=EDGE_CURVE('',#4116,#4124,#2705,.T.);
#4988=ORIENTED_EDGE('',*,*,#4125,.F.);
#4989=ORIENTED_EDGE('',*,*,#4126,.T.);
#4990=ORIENTED_EDGE('',*,*,#4127,.F.);
#4991=ORIENTED_EDGE('',*,*,#4126,.F.);
#4992=ORIENTED_EDGE('',*,*,#4128,.F.);
#4993=ORIENTED_EDGE('',*,*,#4129,.T.);
#4994=ORIENTED_EDGE('',*,*,#4130,.F.);
#4995=ORIENTED_EDGE('',*,*,#4129,.F.);
#4996=ORIENTED_EDGE('',*,*,#4131,.F.);
#4997=ORIENTED_EDGE('',*,*,#4132,.T.);
#4998=ORIENTED_EDGE('',*,*,#4133,.F.);
#4999=ORIENTED_EDGE('',*,*,#4132,.F.);
#5000=ORIENTED_EDGE('',*,*,#4134,.F.);
#5001=ORIENTED_EDGE('',*,*,#4135,.T.);
#5002=ORIENTED_EDGE('',*,*,#4136,.F.);
#5003=ORIENTED_EDGE('',*,*,#4135,.F.);
#5004=ORIENTED_EDGE('',*,*,#4137,.T.);
#5005=ORIENTED_EDGE('',*,*,#4138,.T.);
#5006=ORIENTED_EDGE('',*,*,#4139,.F.);
#5007=ORIENTED_EDGE('',*,*,#4140,.F.);
#5008=ORIENTED_EDGE('',*,*,#4141,.T.);
#5009=ORIENTED_EDGE('',*,*,#4140,.T.);
#5010=ORIENTED_EDGE('',*,*,#4142,.F.);
#5011=ORIENTED_EDGE('',*,*,#4143,.F.);
#5012=ORIENTED_EDGE('',*,*,#4144,.T.);
#5013=ORIENTED_EDGE('',*,*,#4143,.T.);
#5014=ORIENTED_EDGE('',*,*,#4145,.F.);
#5015=ORIENTED_EDGE('',*,*,#4146,.F.);
#5016=ORIENTED_EDGE('',*,*,#4147,.T.);
#5017=ORIENTED_EDGE('',*,*,#4146,.T.);
#5018=ORIENTED_EDGE('',*,*,#4148,.F.);
#5019=ORIENTED_EDGE('',*,*,#4138,.F.);
#5020=ORIENTED_EDGE('',*,*,#4148,.T.);
#5021=ORIENTED_EDGE('',*,*,#4145,.T.);
#5022=ORIENTED_EDGE('',*,*,#4142,.T.);
#5023=ORIENTED_EDGE('',*,*,#4139,.T.);
#5024=ORIENTED_EDGE('',*,*,#4127,.T.);
#5025=ORIENTED_EDGE('',*,*,#4130,.T.);
#5026=ORIENTED_EDGE('',*,*,#4133,.T.);
#5027=ORIENTED_EDGE('',*,*,#4136,.T.);
#5028=ORIENTED_EDGE('',*,*,#4147,.F.);
#5029=ORIENTED_EDGE('',*,*,#4137,.F.);
#5030=ORIENTED_EDGE('',*,*,#4141,.F.);
#5031=ORIENTED_EDGE('',*,*,#4144,.F.);
#5032=ORIENTED_EDGE('',*,*,#4125,.T.);
#5033=ORIENTED_EDGE('',*,*,#4128,.T.);
#5034=ORIENTED_EDGE('',*,*,#4131,.T.);
#5035=ORIENTED_EDGE('',*,*,#4134,.T.);
#5036=ORIENTED_EDGE('',*,*,#4149,.T.);
#5037=ORIENTED_EDGE('',*,*,#4150,.T.);
#5038=ORIENTED_EDGE('',*,*,#4151,.F.);
#5039=ORIENTED_EDGE('',*,*,#4152,.F.);
#5040=ORIENTED_EDGE('',*,*,#4153,.T.);
#5041=ORIENTED_EDGE('',*,*,#4152,.T.);
#5042=ORIENTED_EDGE('',*,*,#4154,.F.);
#5043=ORIENTED_EDGE('',*,*,#4155,.F.);
#5044=ORIENTED_EDGE('',*,*,#4156,.T.);
#5045=ORIENTED_EDGE('',*,*,#4155,.T.);
#5046=ORIENTED_EDGE('',*,*,#4157,.F.);
#5047=ORIENTED_EDGE('',*,*,#4158,.F.);
#5048=ORIENTED_EDGE('',*,*,#4159,.T.);
#5049=ORIENTED_EDGE('',*,*,#4158,.T.);
#5050=ORIENTED_EDGE('',*,*,#4160,.F.);
#5051=ORIENTED_EDGE('',*,*,#4150,.F.);
#5052=ORIENTED_EDGE('',*,*,#4160,.T.);
#5053=ORIENTED_EDGE('',*,*,#4157,.T.);
#5054=ORIENTED_EDGE('',*,*,#4154,.T.);
#5055=ORIENTED_EDGE('',*,*,#4151,.T.);
#5056=ORIENTED_EDGE('',*,*,#4159,.F.);
#5057=ORIENTED_EDGE('',*,*,#4149,.F.);
#5058=ORIENTED_EDGE('',*,*,#4153,.F.);
#5059=ORIENTED_EDGE('',*,*,#4156,.F.);
#5060=ORIENTED_EDGE('',*,*,#4161,.T.);
#5061=ORIENTED_EDGE('',*,*,#4162,.T.);
#5062=ORIENTED_EDGE('',*,*,#4163,.F.);
#5063=ORIENTED_EDGE('',*,*,#4164,.F.);
#5064=ORIENTED_EDGE('',*,*,#4165,.T.);
#5065=ORIENTED_EDGE('',*,*,#4164,.T.);
#5066=ORIENTED_EDGE('',*,*,#4166,.F.);
#5067=ORIENTED_EDGE('',*,*,#4167,.F.);
#5068=ORIENTED_EDGE('',*,*,#4168,.T.);
#5069=ORIENTED_EDGE('',*,*,#4167,.T.);
#5070=ORIENTED_EDGE('',*,*,#4169,.F.);
#5071=ORIENTED_EDGE('',*,*,#4170,.F.);
#5072=ORIENTED_EDGE('',*,*,#4171,.T.);
#5073=ORIENTED_EDGE('',*,*,#4170,.T.);
#5074=ORIENTED_EDGE('',*,*,#4172,.F.);
#5075=ORIENTED_EDGE('',*,*,#4162,.F.);
#5076=ORIENTED_EDGE('',*,*,#4172,.T.);
#5077=ORIENTED_EDGE('',*,*,#4169,.T.);
#5078=ORIENTED_EDGE('',*,*,#4166,.T.);
#5079=ORIENTED_EDGE('',*,*,#4163,.T.);
#5080=ORIENTED_EDGE('',*,*,#4171,.F.);
#5081=ORIENTED_EDGE('',*,*,#4161,.F.);
#5082=ORIENTED_EDGE('',*,*,#4165,.F.);
#5083=ORIENTED_EDGE('',*,*,#4168,.F.);
#5084=ORIENTED_EDGE('',*,*,#4173,.F.);
#5085=ORIENTED_EDGE('',*,*,#4174,.T.);
#5086=ORIENTED_EDGE('',*,*,#4175,.T.);
#5087=ORIENTED_EDGE('',*,*,#4174,.F.);
#5088=ORIENTED_EDGE('',*,*,#4175,.F.);
#5089=ORIENTED_EDGE('',*,*,#4176,.F.);
#5090=ORIENTED_EDGE('',*,*,#4177,.T.);
#5091=ORIENTED_EDGE('',*,*,#4178,.F.);
#5092=ORIENTED_EDGE('',*,*,#4177,.F.);
#5093=ORIENTED_EDGE('',*,*,#4179,.F.);
#5094=ORIENTED_EDGE('',*,*,#4180,.T.);
#5095=ORIENTED_EDGE('',*,*,#4181,.F.);
#5096=ORIENTED_EDGE('',*,*,#4180,.F.);
#5097=ORIENTED_EDGE('',*,*,#4182,.F.);
#5098=ORIENTED_EDGE('',*,*,#4183,.T.);
#5099=ORIENTED_EDGE('',*,*,#4184,.F.);
#5100=ORIENTED_EDGE('',*,*,#4183,.F.);
#5101=ORIENTED_EDGE('',*,*,#4185,.F.);
#5102=ORIENTED_EDGE('',*,*,#4186,.T.);
#5103=ORIENTED_EDGE('',*,*,#4187,.F.);
#5104=ORIENTED_EDGE('',*,*,#4186,.F.);
#5105=ORIENTED_EDGE('',*,*,#4188,.F.);
#5106=ORIENTED_EDGE('',*,*,#4189,.T.);
#5107=ORIENTED_EDGE('',*,*,#4190,.F.);
#5108=ORIENTED_EDGE('',*,*,#4189,.F.);
#5109=ORIENTED_EDGE('',*,*,#4191,.F.);
#5110=ORIENTED_EDGE('',*,*,#4192,.T.);
#5111=ORIENTED_EDGE('',*,*,#4193,.F.);
#5112=ORIENTED_EDGE('',*,*,#4192,.F.);
#5113=ORIENTED_EDGE('',*,*,#4194,.F.);
#5114=ORIENTED_EDGE('',*,*,#4195,.T.);
#5115=ORIENTED_EDGE('',*,*,#4196,.F.);
#5116=ORIENTED_EDGE('',*,*,#4195,.F.);
#5117=ORIENTED_EDGE('',*,*,#4197,.F.);
#5118=ORIENTED_EDGE('',*,*,#4198,.T.);
#5119=ORIENTED_EDGE('',*,*,#4199,.F.);
#5120=ORIENTED_EDGE('',*,*,#4198,.F.);
#5121=ORIENTED_EDGE('',*,*,#4200,.F.);
#5122=ORIENTED_EDGE('',*,*,#4201,.T.);
#5123=ORIENTED_EDGE('',*,*,#4202,.F.);
#5124=ORIENTED_EDGE('',*,*,#4201,.F.);
#5125=ORIENTED_EDGE('',*,*,#4203,.F.);
#5126=ORIENTED_EDGE('',*,*,#4204,.T.);
#5127=ORIENTED_EDGE('',*,*,#4205,.F.);
#5128=ORIENTED_EDGE('',*,*,#4204,.F.);
#5129=ORIENTED_EDGE('',*,*,#4206,.F.);
#5130=ORIENTED_EDGE('',*,*,#4207,.T.);
#5131=ORIENTED_EDGE('',*,*,#4208,.F.);
#5132=ORIENTED_EDGE('',*,*,#4207,.F.);
#5133=ORIENTED_EDGE('',*,*,#4209,.F.);
#5134=ORIENTED_EDGE('',*,*,#4210,.T.);
#5135=ORIENTED_EDGE('',*,*,#4211,.F.);
#5136=ORIENTED_EDGE('',*,*,#4210,.F.);
#5137=ORIENTED_EDGE('',*,*,#4212,.F.);
#5138=ORIENTED_EDGE('',*,*,#4213,.F.);
#5139=ORIENTED_EDGE('',*,*,#4214,.F.);
#5140=ORIENTED_EDGE('',*,*,#4215,.F.);
#5141=ORIENTED_EDGE('',*,*,#4216,.T.);
#5142=ORIENTED_EDGE('',*,*,#4217,.F.);
#5143=ORIENTED_EDGE('',*,*,#4218,.F.);
#5144=ORIENTED_EDGE('',*,*,#4219,.F.);
#5145=ORIENTED_EDGE('',*,*,#4202,.T.);
#5146=ORIENTED_EDGE('',*,*,#4205,.T.);
#5147=ORIENTED_EDGE('',*,*,#4208,.T.);
#5148=ORIENTED_EDGE('',*,*,#4211,.T.);
#5149=ORIENTED_EDGE('',*,*,#4220,.F.);
#5150=ORIENTED_EDGE('',*,*,#4218,.T.);
#5151=ORIENTED_EDGE('',*,*,#4221,.F.);
#5152=ORIENTED_EDGE('',*,*,#4222,.F.);
#5153=ORIENTED_EDGE('',*,*,#4223,.F.);
#5154=ORIENTED_EDGE('',*,*,#4222,.T.);
#5155=ORIENTED_EDGE('',*,*,#4224,.F.);
#5156=ORIENTED_EDGE('',*,*,#4225,.F.);
#5157=ORIENTED_EDGE('',*,*,#4200,.T.);
#5158=ORIENTED_EDGE('',*,*,#4203,.T.);
#5159=ORIENTED_EDGE('',*,*,#4206,.T.);
#5160=ORIENTED_EDGE('',*,*,#4209,.T.);
#5161=ORIENTED_EDGE('',*,*,#4226,.F.);
#5162=ORIENTED_EDGE('',*,*,#4225,.T.);
#5163=ORIENTED_EDGE('',*,*,#4227,.F.);
#5164=ORIENTED_EDGE('',*,*,#4216,.F.);
#5165=ORIENTED_EDGE('',*,*,#4217,.T.);
#5166=ORIENTED_EDGE('',*,*,#4227,.T.);
#5167=ORIENTED_EDGE('',*,*,#4224,.T.);
#5168=ORIENTED_EDGE('',*,*,#4221,.T.);
#5169=ORIENTED_EDGE('',*,*,#4213,.T.);
#5170=ORIENTED_EDGE('',*,*,#4228,.T.);
#5171=ORIENTED_EDGE('',*,*,#4229,.F.);
#5172=ORIENTED_EDGE('',*,*,#4230,.F.);
#5173=ORIENTED_EDGE('',*,*,#4199,.T.);
#5174=ORIENTED_EDGE('',*,*,#4196,.T.);
#5175=ORIENTED_EDGE('',*,*,#4193,.T.);
#5176=ORIENTED_EDGE('',*,*,#4190,.T.);
#5177=ORIENTED_EDGE('',*,*,#4187,.T.);
#5178=ORIENTED_EDGE('',*,*,#4184,.T.);
#5179=ORIENTED_EDGE('',*,*,#4181,.T.);
#5180=ORIENTED_EDGE('',*,*,#4178,.T.);
#5181=ORIENTED_EDGE('',*,*,#4214,.T.);
#5182=ORIENTED_EDGE('',*,*,#4230,.T.);
#5183=ORIENTED_EDGE('',*,*,#4231,.F.);
#5184=ORIENTED_EDGE('',*,*,#4232,.F.);
#5185=ORIENTED_EDGE('',*,*,#4232,.T.);
#5186=ORIENTED_EDGE('',*,*,#4233,.F.);
#5187=ORIENTED_EDGE('',*,*,#4234,.F.);
#5188=ORIENTED_EDGE('',*,*,#4219,.T.);
#5189=ORIENTED_EDGE('',*,*,#4220,.T.);
#5190=ORIENTED_EDGE('',*,*,#4223,.T.);
#5191=ORIENTED_EDGE('',*,*,#4226,.T.);
#5192=ORIENTED_EDGE('',*,*,#4215,.T.);
#5193=ORIENTED_EDGE('',*,*,#4197,.T.);
#5194=ORIENTED_EDGE('',*,*,#4194,.T.);
#5195=ORIENTED_EDGE('',*,*,#4191,.T.);
#5196=ORIENTED_EDGE('',*,*,#4188,.T.);
#5197=ORIENTED_EDGE('',*,*,#4185,.T.);
#5198=ORIENTED_EDGE('',*,*,#4182,.T.);
#5199=ORIENTED_EDGE('',*,*,#4179,.T.);
#5200=ORIENTED_EDGE('',*,*,#4176,.T.);
#5201=ORIENTED_EDGE('',*,*,#4212,.T.);
#5202=ORIENTED_EDGE('',*,*,#4234,.T.);
#5203=ORIENTED_EDGE('',*,*,#4235,.F.);
#5204=ORIENTED_EDGE('',*,*,#4228,.F.);
#5205=ORIENTED_EDGE('',*,*,#4173,.T.);
#5206=ORIENTED_EDGE('',*,*,#4235,.T.);
#5207=ORIENTED_EDGE('',*,*,#4233,.T.);
#5208=ORIENTED_EDGE('',*,*,#4231,.T.);
#5209=ORIENTED_EDGE('',*,*,#4229,.T.);
#5210=ORIENTED_EDGE('',*,*,#4236,.F.);
#5211=ORIENTED_EDGE('',*,*,#4237,.T.);
#5212=ORIENTED_EDGE('',*,*,#4238,.T.);
#5213=ORIENTED_EDGE('',*,*,#4237,.F.);
#5214=ORIENTED_EDGE('',*,*,#4238,.F.);
#5215=ORIENTED_EDGE('',*,*,#4239,.F.);
#5216=ORIENTED_EDGE('',*,*,#4240,.T.);
#5217=ORIENTED_EDGE('',*,*,#4241,.F.);
#5218=ORIENTED_EDGE('',*,*,#4240,.F.);
#5219=ORIENTED_EDGE('',*,*,#4242,.F.);
#5220=ORIENTED_EDGE('',*,*,#4243,.T.);
#5221=ORIENTED_EDGE('',*,*,#4244,.F.);
#5222=ORIENTED_EDGE('',*,*,#4243,.F.);
#5223=ORIENTED_EDGE('',*,*,#4245,.F.);
#5224=ORIENTED_EDGE('',*,*,#4246,.T.);
#5225=ORIENTED_EDGE('',*,*,#4247,.F.);
#5226=ORIENTED_EDGE('',*,*,#4246,.F.);
#5227=ORIENTED_EDGE('',*,*,#4248,.T.);
#5228=ORIENTED_EDGE('',*,*,#4241,.T.);
#5229=ORIENTED_EDGE('',*,*,#4244,.T.);
#5230=ORIENTED_EDGE('',*,*,#4247,.T.);
#5231=ORIENTED_EDGE('',*,*,#4249,.F.);
#5232=ORIENTED_EDGE('',*,*,#4250,.F.);
#5233=ORIENTED_EDGE('',*,*,#4239,.T.);
#5234=ORIENTED_EDGE('',*,*,#4242,.T.);
#5235=ORIENTED_EDGE('',*,*,#4245,.T.);
#5236=ORIENTED_EDGE('',*,*,#4251,.F.);
#5237=ORIENTED_EDGE('',*,*,#4248,.F.);
#5238=ORIENTED_EDGE('',*,*,#4252,.T.);
#5239=ORIENTED_EDGE('',*,*,#4250,.T.);
#5240=ORIENTED_EDGE('',*,*,#4252,.F.);
#5241=ORIENTED_EDGE('',*,*,#4251,.T.);
#5242=ORIENTED_EDGE('',*,*,#4253,.T.);
#5243=ORIENTED_EDGE('',*,*,#4254,.T.);
#5244=ORIENTED_EDGE('',*,*,#4253,.F.);
#5245=ORIENTED_EDGE('',*,*,#4255,.F.);
#5246=ORIENTED_EDGE('',*,*,#4256,.T.);
#5247=ORIENTED_EDGE('',*,*,#4249,.T.);
#5248=ORIENTED_EDGE('',*,*,#4256,.F.);
#5249=ORIENTED_EDGE('',*,*,#4255,.T.);
#5250=ORIENTED_EDGE('',*,*,#4254,.F.);
#5251=ORIENTED_EDGE('',*,*,#4236,.T.);
#5252=ORIENTED_EDGE('',*,*,#4257,.F.);
#5253=ORIENTED_EDGE('',*,*,#4258,.T.);
#5254=ORIENTED_EDGE('',*,*,#4259,.T.);
#5255=ORIENTED_EDGE('',*,*,#4258,.F.);
#5256=ORIENTED_EDGE('',*,*,#4260,.F.);
#5257=ORIENTED_EDGE('',*,*,#4261,.T.);
#5258=ORIENTED_EDGE('',*,*,#4262,.T.);
#5259=ORIENTED_EDGE('',*,*,#4261,.F.);
#5260=ORIENTED_EDGE('',*,*,#4260,.T.);
#5261=ORIENTED_EDGE('',*,*,#4257,.T.);
#5262=ORIENTED_EDGE('',*,*,#4262,.F.);
#5263=ORIENTED_EDGE('',*,*,#4259,.F.);
#5264=ORIENTED_EDGE('',*,*,#4263,.F.);
#5265=ORIENTED_EDGE('',*,*,#4264,.T.);
#5266=ORIENTED_EDGE('',*,*,#4265,.T.);
#5267=ORIENTED_EDGE('',*,*,#4264,.F.);
#5268=ORIENTED_EDGE('',*,*,#4266,.F.);
#5269=ORIENTED_EDGE('',*,*,#4267,.T.);
#5270=ORIENTED_EDGE('',*,*,#4268,.T.);
#5271=ORIENTED_EDGE('',*,*,#4267,.F.);
#5272=ORIENTED_EDGE('',*,*,#4266,.T.);
#5273=ORIENTED_EDGE('',*,*,#4263,.T.);
#5274=ORIENTED_EDGE('',*,*,#4268,.F.);
#5275=ORIENTED_EDGE('',*,*,#4265,.F.);
#5276=ORIENTED_EDGE('',*,*,#4269,.F.);
#5277=ORIENTED_EDGE('',*,*,#4270,.T.);
#5278=ORIENTED_EDGE('',*,*,#4271,.T.);
#5279=ORIENTED_EDGE('',*,*,#4270,.F.);
#5280=ORIENTED_EDGE('',*,*,#4272,.F.);
#5281=ORIENTED_EDGE('',*,*,#4273,.T.);
#5282=ORIENTED_EDGE('',*,*,#4274,.T.);
#5283=ORIENTED_EDGE('',*,*,#4273,.F.);
#5284=ORIENTED_EDGE('',*,*,#4272,.T.);
#5285=ORIENTED_EDGE('',*,*,#4269,.T.);
#5286=ORIENTED_EDGE('',*,*,#4274,.F.);
#5287=ORIENTED_EDGE('',*,*,#4271,.F.);
#5288=ORIENTED_EDGE('',*,*,#4275,.F.);
#5289=ORIENTED_EDGE('',*,*,#4276,.T.);
#5290=ORIENTED_EDGE('',*,*,#4277,.T.);
#5291=ORIENTED_EDGE('',*,*,#4276,.F.);
#5292=ORIENTED_EDGE('',*,*,#4278,.F.);
#5293=ORIENTED_EDGE('',*,*,#4279,.T.);
#5294=ORIENTED_EDGE('',*,*,#4280,.T.);
#5295=ORIENTED_EDGE('',*,*,#4279,.F.);
#5296=ORIENTED_EDGE('',*,*,#4278,.T.);
#5297=ORIENTED_EDGE('',*,*,#4275,.T.);
#5298=ORIENTED_EDGE('',*,*,#4280,.F.);
#5299=ORIENTED_EDGE('',*,*,#4277,.F.);
#5300=ORIENTED_EDGE('',*,*,#4281,.F.);
#5301=ORIENTED_EDGE('',*,*,#4282,.T.);
#5302=ORIENTED_EDGE('',*,*,#4283,.T.);
#5303=ORIENTED_EDGE('',*,*,#4282,.F.);
#5304=ORIENTED_EDGE('',*,*,#4283,.F.);
#5305=ORIENTED_EDGE('',*,*,#4284,.F.);
#5306=ORIENTED_EDGE('',*,*,#4285,.T.);
#5307=ORIENTED_EDGE('',*,*,#4286,.F.);
#5308=ORIENTED_EDGE('',*,*,#4285,.F.);
#5309=ORIENTED_EDGE('',*,*,#4287,.F.);
#5310=ORIENTED_EDGE('',*,*,#4288,.T.);
#5311=ORIENTED_EDGE('',*,*,#4289,.F.);
#5312=ORIENTED_EDGE('',*,*,#4288,.F.);
#5313=ORIENTED_EDGE('',*,*,#4290,.F.);
#5314=ORIENTED_EDGE('',*,*,#4291,.T.);
#5315=ORIENTED_EDGE('',*,*,#4292,.F.);
#5316=ORIENTED_EDGE('',*,*,#4291,.F.);
#5317=ORIENTED_EDGE('',*,*,#4293,.T.);
#5318=ORIENTED_EDGE('',*,*,#4286,.T.);
#5319=ORIENTED_EDGE('',*,*,#4289,.T.);
#5320=ORIENTED_EDGE('',*,*,#4292,.T.);
#5321=ORIENTED_EDGE('',*,*,#4294,.F.);
#5322=ORIENTED_EDGE('',*,*,#4295,.F.);
#5323=ORIENTED_EDGE('',*,*,#4284,.T.);
#5324=ORIENTED_EDGE('',*,*,#4287,.T.);
#5325=ORIENTED_EDGE('',*,*,#4290,.T.);
#5326=ORIENTED_EDGE('',*,*,#4296,.F.);
#5327=ORIENTED_EDGE('',*,*,#4293,.F.);
#5328=ORIENTED_EDGE('',*,*,#4297,.T.);
#5329=ORIENTED_EDGE('',*,*,#4295,.T.);
#5330=ORIENTED_EDGE('',*,*,#4297,.F.);
#5331=ORIENTED_EDGE('',*,*,#4296,.T.);
#5332=ORIENTED_EDGE('',*,*,#4298,.T.);
#5333=ORIENTED_EDGE('',*,*,#4299,.T.);
#5334=ORIENTED_EDGE('',*,*,#4298,.F.);
#5335=ORIENTED_EDGE('',*,*,#4300,.F.);
#5336=ORIENTED_EDGE('',*,*,#4301,.T.);
#5337=ORIENTED_EDGE('',*,*,#4294,.T.);
#5338=ORIENTED_EDGE('',*,*,#4301,.F.);
#5339=ORIENTED_EDGE('',*,*,#4300,.T.);
#5340=ORIENTED_EDGE('',*,*,#4299,.F.);
#5341=ORIENTED_EDGE('',*,*,#4281,.T.);
#5342=ORIENTED_EDGE('',*,*,#4302,.F.);
#5343=ORIENTED_EDGE('',*,*,#4303,.T.);
#5344=ORIENTED_EDGE('',*,*,#4304,.T.);
#5345=ORIENTED_EDGE('',*,*,#4303,.F.);
#5346=ORIENTED_EDGE('',*,*,#4305,.F.);
#5347=ORIENTED_EDGE('',*,*,#4306,.T.);
#5348=ORIENTED_EDGE('',*,*,#4307,.T.);
#5349=ORIENTED_EDGE('',*,*,#4306,.F.);
#5350=ORIENTED_EDGE('',*,*,#4305,.T.);
#5351=ORIENTED_EDGE('',*,*,#4302,.T.);
#5352=ORIENTED_EDGE('',*,*,#4307,.F.);
#5353=ORIENTED_EDGE('',*,*,#4304,.F.);
#5354=ORIENTED_EDGE('',*,*,#4308,.F.);
#5355=ORIENTED_EDGE('',*,*,#4309,.T.);
#5356=ORIENTED_EDGE('',*,*,#4310,.T.);
#5357=ORIENTED_EDGE('',*,*,#4309,.F.);
#5358=ORIENTED_EDGE('',*,*,#4311,.F.);
#5359=ORIENTED_EDGE('',*,*,#4312,.T.);
#5360=ORIENTED_EDGE('',*,*,#4313,.T.);
#5361=ORIENTED_EDGE('',*,*,#4312,.F.);
#5362=ORIENTED_EDGE('',*,*,#4311,.T.);
#5363=ORIENTED_EDGE('',*,*,#4308,.T.);
#5364=ORIENTED_EDGE('',*,*,#4313,.F.);
#5365=ORIENTED_EDGE('',*,*,#4310,.F.);
#5366=ORIENTED_EDGE('',*,*,#4314,.F.);
#5367=ORIENTED_EDGE('',*,*,#4315,.T.);
#5368=ORIENTED_EDGE('',*,*,#4316,.T.);
#5369=ORIENTED_EDGE('',*,*,#4315,.F.);
#5370=ORIENTED_EDGE('',*,*,#4317,.F.);
#5371=ORIENTED_EDGE('',*,*,#4318,.T.);
#5372=ORIENTED_EDGE('',*,*,#4319,.T.);
#5373=ORIENTED_EDGE('',*,*,#4318,.F.);
#5374=ORIENTED_EDGE('',*,*,#4317,.T.);
#5375=ORIENTED_EDGE('',*,*,#4314,.T.);
#5376=ORIENTED_EDGE('',*,*,#4319,.F.);
#5377=ORIENTED_EDGE('',*,*,#4316,.F.);
#5378=ORIENTED_EDGE('',*,*,#4320,.F.);
#5379=ORIENTED_EDGE('',*,*,#4321,.T.);
#5380=ORIENTED_EDGE('',*,*,#4322,.T.);
#5381=ORIENTED_EDGE('',*,*,#4321,.F.);
#5382=ORIENTED_EDGE('',*,*,#4323,.F.);
#5383=ORIENTED_EDGE('',*,*,#4324,.T.);
#5384=ORIENTED_EDGE('',*,*,#4325,.T.);
#5385=ORIENTED_EDGE('',*,*,#4324,.F.);
#5386=ORIENTED_EDGE('',*,*,#4323,.T.);
#5387=ORIENTED_EDGE('',*,*,#4320,.T.);
#5388=ORIENTED_EDGE('',*,*,#4325,.F.);
#5389=ORIENTED_EDGE('',*,*,#4322,.F.);
#5390=ORIENTED_EDGE('',*,*,#4326,.F.);
#5391=ORIENTED_EDGE('',*,*,#4327,.T.);
#5392=ORIENTED_EDGE('',*,*,#4328,.F.);
#5393=ORIENTED_EDGE('',*,*,#4327,.F.);
#5394=ORIENTED_EDGE('',*,*,#4329,.F.);
#5395=ORIENTED_EDGE('',*,*,#4330,.T.);
#5396=ORIENTED_EDGE('',*,*,#4331,.F.);
#5397=ORIENTED_EDGE('',*,*,#4330,.F.);
#5398=ORIENTED_EDGE('',*,*,#4332,.F.);
#5399=ORIENTED_EDGE('',*,*,#4333,.F.);
#5400=ORIENTED_EDGE('',*,*,#4334,.T.);
#5401=ORIENTED_EDGE('',*,*,#4335,.F.);
#5402=ORIENTED_EDGE('',*,*,#4336,.F.);
#5403=ORIENTED_EDGE('',*,*,#4337,.T.);
#5404=ORIENTED_EDGE('',*,*,#4338,.F.);
#5405=ORIENTED_EDGE('',*,*,#4334,.F.);
#5406=ORIENTED_EDGE('',*,*,#4331,.T.);
#5407=ORIENTED_EDGE('',*,*,#4339,.T.);
#5408=ORIENTED_EDGE('',*,*,#4340,.T.);
#5409=ORIENTED_EDGE('',*,*,#4341,.F.);
#5410=ORIENTED_EDGE('',*,*,#4342,.F.);
#5411=ORIENTED_EDGE('',*,*,#4343,.T.);
#5412=ORIENTED_EDGE('',*,*,#4344,.T.);
#5413=ORIENTED_EDGE('',*,*,#4336,.T.);
#5414=ORIENTED_EDGE('',*,*,#4333,.T.);
#5415=ORIENTED_EDGE('',*,*,#4332,.T.);
#5416=ORIENTED_EDGE('',*,*,#4345,.F.);
#5417=ORIENTED_EDGE('',*,*,#4346,.F.);
#5418=ORIENTED_EDGE('',*,*,#4339,.F.);
#5419=ORIENTED_EDGE('',*,*,#4347,.T.);
#5420=ORIENTED_EDGE('',*,*,#4348,.F.);
#5421=ORIENTED_EDGE('',*,*,#4345,.T.);
#5422=ORIENTED_EDGE('',*,*,#4335,.T.);
#5423=ORIENTED_EDGE('',*,*,#4338,.T.);
#5424=ORIENTED_EDGE('',*,*,#4349,.T.);
#5425=ORIENTED_EDGE('',*,*,#4344,.F.);
#5426=ORIENTED_EDGE('',*,*,#4350,.T.);
#5427=ORIENTED_EDGE('',*,*,#4349,.F.);
#5428=ORIENTED_EDGE('',*,*,#4337,.F.);
#5429=ORIENTED_EDGE('',*,*,#4351,.T.);
#5430=ORIENTED_EDGE('',*,*,#4342,.T.);
#5431=ORIENTED_EDGE('',*,*,#4352,.F.);
#5432=ORIENTED_EDGE('',*,*,#4353,.F.);
#5433=ORIENTED_EDGE('',*,*,#4326,.T.);
#5434=ORIENTED_EDGE('',*,*,#4354,.T.);
#5435=ORIENTED_EDGE('',*,*,#4353,.T.);
#5436=ORIENTED_EDGE('',*,*,#4355,.F.);
#5437=ORIENTED_EDGE('',*,*,#4356,.F.);
#5438=ORIENTED_EDGE('',*,*,#4348,.T.);
#5439=ORIENTED_EDGE('',*,*,#4357,.T.);
#5440=ORIENTED_EDGE('',*,*,#4356,.T.);
#5441=ORIENTED_EDGE('',*,*,#4358,.F.);
#5442=ORIENTED_EDGE('',*,*,#4340,.F.);
#5443=ORIENTED_EDGE('',*,*,#4346,.T.);
#5444=ORIENTED_EDGE('',*,*,#4328,.T.);
#5445=ORIENTED_EDGE('',*,*,#4352,.T.);
#5446=ORIENTED_EDGE('',*,*,#4341,.T.);
#5447=ORIENTED_EDGE('',*,*,#4358,.T.);
#5448=ORIENTED_EDGE('',*,*,#4355,.T.);
#5449=ORIENTED_EDGE('',*,*,#4343,.F.);
#5450=ORIENTED_EDGE('',*,*,#4351,.F.);
#5451=ORIENTED_EDGE('',*,*,#4354,.F.);
#5452=ORIENTED_EDGE('',*,*,#4357,.F.);
#5453=ORIENTED_EDGE('',*,*,#4347,.F.);
#5454=ORIENTED_EDGE('',*,*,#4350,.F.);
#5455=ORIENTED_EDGE('',*,*,#4329,.T.);
#5456=ORIENTED_EDGE('',*,*,#4359,.F.);
#5457=ORIENTED_EDGE('',*,*,#4360,.T.);
#5458=ORIENTED_EDGE('',*,*,#4361,.T.);
#5459=ORIENTED_EDGE('',*,*,#4362,.F.);
#5460=ORIENTED_EDGE('',*,*,#4363,.F.);
#5461=ORIENTED_EDGE('',*,*,#4364,.T.);
#5462=ORIENTED_EDGE('',*,*,#4360,.F.);
#5463=ORIENTED_EDGE('',*,*,#4359,.T.);
#5464=ORIENTED_EDGE('',*,*,#4365,.F.);
#5465=ORIENTED_EDGE('',*,*,#4361,.F.);
#5466=ORIENTED_EDGE('',*,*,#4364,.F.);
#5467=ORIENTED_EDGE('',*,*,#4365,.T.);
#5468=ORIENTED_EDGE('',*,*,#4366,.T.);
#5469=ORIENTED_EDGE('',*,*,#4367,.F.);
#5470=ORIENTED_EDGE('',*,*,#4368,.T.);
#5471=ORIENTED_EDGE('',*,*,#4369,.F.);
#5472=ORIENTED_EDGE('',*,*,#4370,.T.);
#5473=ORIENTED_EDGE('',*,*,#4371,.F.);
#5474=ORIENTED_EDGE('',*,*,#4372,.F.);
#5475=ORIENTED_EDGE('',*,*,#4368,.F.);
#5476=ORIENTED_EDGE('',*,*,#4367,.T.);
#5477=ORIENTED_EDGE('',*,*,#4373,.F.);
#5478=ORIENTED_EDGE('',*,*,#4370,.F.);
#5479=ORIENTED_EDGE('',*,*,#4373,.T.);
#5480=ORIENTED_EDGE('',*,*,#4374,.F.);
#5481=ORIENTED_EDGE('',*,*,#4362,.T.);
#5482=ORIENTED_EDGE('',*,*,#4366,.F.);
#5483=ORIENTED_EDGE('',*,*,#4363,.T.);
#5484=ORIENTED_EDGE('',*,*,#4375,.F.);
#5485=ORIENTED_EDGE('',*,*,#4371,.T.);
#5486=ORIENTED_EDGE('',*,*,#4374,.T.);
#5487=ORIENTED_EDGE('',*,*,#4369,.T.);
#5488=ORIENTED_EDGE('',*,*,#4372,.T.);
#5489=ORIENTED_EDGE('',*,*,#4375,.T.);
#5490=ORIENTED_EDGE('',*,*,#4376,.T.);
#5491=ORIENTED_EDGE('',*,*,#4377,.T.);
#5492=ORIENTED_EDGE('',*,*,#4378,.T.);
#5493=ORIENTED_EDGE('',*,*,#4379,.F.);
#5494=ORIENTED_EDGE('',*,*,#4380,.T.);
#5495=ORIENTED_EDGE('',*,*,#4381,.T.);
#5496=ORIENTED_EDGE('',*,*,#4382,.T.);
#5497=ORIENTED_EDGE('',*,*,#4377,.F.);
#5498=ORIENTED_EDGE('',*,*,#4383,.T.);
#5499=ORIENTED_EDGE('',*,*,#4384,.T.);
#5500=ORIENTED_EDGE('',*,*,#4385,.T.);
#5501=ORIENTED_EDGE('',*,*,#4381,.F.);
#5502=ORIENTED_EDGE('',*,*,#4386,.T.);
#5503=ORIENTED_EDGE('',*,*,#4387,.T.);
#5504=ORIENTED_EDGE('',*,*,#4388,.T.);
#5505=ORIENTED_EDGE('',*,*,#4384,.F.);
#5506=ORIENTED_EDGE('',*,*,#4389,.T.);
#5507=ORIENTED_EDGE('',*,*,#4390,.T.);
#5508=ORIENTED_EDGE('',*,*,#4391,.T.);
#5509=ORIENTED_EDGE('',*,*,#4387,.F.);
#5510=ORIENTED_EDGE('',*,*,#4392,.T.);
#5511=ORIENTED_EDGE('',*,*,#4379,.T.);
#5512=ORIENTED_EDGE('',*,*,#4393,.T.);
#5513=ORIENTED_EDGE('',*,*,#4390,.F.);
#5514=ORIENTED_EDGE('',*,*,#4392,.F.);
#5515=ORIENTED_EDGE('',*,*,#4389,.F.);
#5516=ORIENTED_EDGE('',*,*,#4386,.F.);
#5517=ORIENTED_EDGE('',*,*,#4383,.F.);
#5518=ORIENTED_EDGE('',*,*,#4380,.F.);
#5519=ORIENTED_EDGE('',*,*,#4376,.F.);
#5520=ORIENTED_EDGE('',*,*,#4393,.F.);
#5521=ORIENTED_EDGE('',*,*,#4378,.F.);
#5522=ORIENTED_EDGE('',*,*,#4382,.F.);
#5523=ORIENTED_EDGE('',*,*,#4385,.F.);
#5524=ORIENTED_EDGE('',*,*,#4388,.F.);
#5525=ORIENTED_EDGE('',*,*,#4391,.F.);
#5526=ORIENTED_EDGE('',*,*,#4394,.F.);
#5527=ORIENTED_EDGE('',*,*,#4395,.F.);
#5528=ORIENTED_EDGE('',*,*,#4396,.F.);
#5529=ORIENTED_EDGE('',*,*,#4397,.T.);
#5530=ORIENTED_EDGE('',*,*,#4395,.T.);
#5531=ORIENTED_EDGE('',*,*,#4397,.F.);
#5532=ORIENTED_EDGE('',*,*,#4398,.F.);
#5533=ORIENTED_EDGE('',*,*,#4399,.T.);
#5534=ORIENTED_EDGE('',*,*,#4396,.T.);
#5535=ORIENTED_EDGE('',*,*,#4399,.F.);
#5536=ORIENTED_EDGE('',*,*,#4400,.F.);
#5537=ORIENTED_EDGE('',*,*,#4401,.T.);
#5538=ORIENTED_EDGE('',*,*,#4398,.T.);
#5539=ORIENTED_EDGE('',*,*,#4401,.F.);
#5540=ORIENTED_EDGE('',*,*,#4400,.T.);
#5541=ORIENTED_EDGE('',*,*,#4402,.F.);
#5542=ORIENTED_EDGE('',*,*,#4403,.F.);
#5543=ORIENTED_EDGE('',*,*,#4404,.T.);
#5544=ORIENTED_EDGE('',*,*,#4402,.T.);
#5545=ORIENTED_EDGE('',*,*,#4404,.F.);
#5546=ORIENTED_EDGE('',*,*,#4394,.T.);
#5547=ORIENTED_EDGE('',*,*,#4405,.T.);
#5548=ORIENTED_EDGE('',*,*,#4403,.T.);
#5549=ORIENTED_EDGE('',*,*,#4405,.F.);
#5550=ORIENTED_EDGE('',*,*,#4406,.F.);
#5551=ORIENTED_EDGE('',*,*,#4407,.T.);
#5552=ORIENTED_EDGE('',*,*,#4408,.F.);
#5553=ORIENTED_EDGE('',*,*,#4407,.F.);
#5554=ORIENTED_EDGE('',*,*,#4409,.F.);
#5555=ORIENTED_EDGE('',*,*,#4410,.T.);
#5556=ORIENTED_EDGE('',*,*,#4411,.F.);
#5557=ORIENTED_EDGE('',*,*,#4410,.F.);
#5558=ORIENTED_EDGE('',*,*,#4412,.F.);
#5559=ORIENTED_EDGE('',*,*,#4413,.T.);
#5560=ORIENTED_EDGE('',*,*,#4414,.F.);
#5561=ORIENTED_EDGE('',*,*,#4413,.F.);
#5562=ORIENTED_EDGE('',*,*,#4415,.F.);
#5563=ORIENTED_EDGE('',*,*,#4416,.T.);
#5564=ORIENTED_EDGE('',*,*,#4417,.F.);
#5565=ORIENTED_EDGE('',*,*,#4416,.F.);
#5566=ORIENTED_EDGE('',*,*,#4418,.F.);
#5567=ORIENTED_EDGE('',*,*,#4419,.T.);
#5568=ORIENTED_EDGE('',*,*,#4420,.F.);
#5569=ORIENTED_EDGE('',*,*,#4419,.F.);
#5570=ORIENTED_EDGE('',*,*,#4421,.F.);
#5571=ORIENTED_EDGE('',*,*,#4422,.T.);
#5572=ORIENTED_EDGE('',*,*,#4423,.F.);
#5573=ORIENTED_EDGE('',*,*,#4422,.F.);
#5574=ORIENTED_EDGE('',*,*,#4424,.F.);
#5575=ORIENTED_EDGE('',*,*,#4425,.T.);
#5576=ORIENTED_EDGE('',*,*,#4426,.F.);
#5577=ORIENTED_EDGE('',*,*,#4425,.F.);
#5578=ORIENTED_EDGE('',*,*,#4427,.F.);
#5579=ORIENTED_EDGE('',*,*,#4428,.T.);
#5580=ORIENTED_EDGE('',*,*,#4429,.F.);
#5581=ORIENTED_EDGE('',*,*,#4428,.F.);
#5582=ORIENTED_EDGE('',*,*,#4430,.F.);
#5583=ORIENTED_EDGE('',*,*,#4431,.T.);
#5584=ORIENTED_EDGE('',*,*,#4432,.F.);
#5585=ORIENTED_EDGE('',*,*,#4431,.F.);
#5586=ORIENTED_EDGE('',*,*,#4433,.F.);
#5587=ORIENTED_EDGE('',*,*,#4434,.T.);
#5588=ORIENTED_EDGE('',*,*,#4435,.F.);
#5589=ORIENTED_EDGE('',*,*,#4434,.F.);
#5590=ORIENTED_EDGE('',*,*,#4436,.F.);
#5591=ORIENTED_EDGE('',*,*,#4437,.F.);
#5592=ORIENTED_EDGE('',*,*,#4438,.F.);
#5593=ORIENTED_EDGE('',*,*,#4439,.T.);
#5594=ORIENTED_EDGE('',*,*,#4436,.T.);
#5595=ORIENTED_EDGE('',*,*,#4440,.F.);
#5596=ORIENTED_EDGE('',*,*,#4441,.F.);
#5597=ORIENTED_EDGE('',*,*,#4442,.F.);
#5598=ORIENTED_EDGE('',*,*,#4439,.F.);
#5599=ORIENTED_EDGE('',*,*,#4443,.T.);
#5600=ORIENTED_EDGE('',*,*,#4444,.F.);
#5601=ORIENTED_EDGE('',*,*,#4440,.T.);
#5602=ORIENTED_EDGE('',*,*,#4418,.T.);
#5603=ORIENTED_EDGE('',*,*,#4421,.T.);
#5604=ORIENTED_EDGE('',*,*,#4424,.T.);
#5605=ORIENTED_EDGE('',*,*,#4427,.T.);
#5606=ORIENTED_EDGE('',*,*,#4430,.T.);
#5607=ORIENTED_EDGE('',*,*,#4433,.T.);
#5608=ORIENTED_EDGE('',*,*,#4415,.T.);
#5609=ORIENTED_EDGE('',*,*,#4412,.T.);
#5610=ORIENTED_EDGE('',*,*,#4409,.T.);
#5611=ORIENTED_EDGE('',*,*,#4406,.T.);
#5612=ORIENTED_EDGE('',*,*,#4438,.T.);
#5613=ORIENTED_EDGE('',*,*,#4445,.F.);
#5614=ORIENTED_EDGE('',*,*,#4446,.F.);
#5615=ORIENTED_EDGE('',*,*,#4443,.F.);
#5616=ORIENTED_EDGE('',*,*,#4441,.T.);
#5617=ORIENTED_EDGE('',*,*,#4444,.T.);
#5618=ORIENTED_EDGE('',*,*,#4446,.T.);
#5619=ORIENTED_EDGE('',*,*,#4447,.F.);
#5620=ORIENTED_EDGE('',*,*,#4442,.T.);
#5621=ORIENTED_EDGE('',*,*,#4447,.T.);
#5622=ORIENTED_EDGE('',*,*,#4445,.T.);
#5623=ORIENTED_EDGE('',*,*,#4437,.T.);
#5624=ORIENTED_EDGE('',*,*,#4420,.T.);
#5625=ORIENTED_EDGE('',*,*,#4423,.T.);
#5626=ORIENTED_EDGE('',*,*,#4426,.T.);
#5627=ORIENTED_EDGE('',*,*,#4429,.T.);
#5628=ORIENTED_EDGE('',*,*,#4432,.T.);
#5629=ORIENTED_EDGE('',*,*,#4435,.T.);
#5630=ORIENTED_EDGE('',*,*,#4417,.T.);
#5631=ORIENTED_EDGE('',*,*,#4414,.T.);
#5632=ORIENTED_EDGE('',*,*,#4411,.T.);
#5633=ORIENTED_EDGE('',*,*,#4408,.T.);
#5634=ORIENTED_EDGE('',*,*,#4448,.F.);
#5635=ORIENTED_EDGE('',*,*,#4449,.T.);
#5636=ORIENTED_EDGE('',*,*,#4450,.T.);
#5637=ORIENTED_EDGE('',*,*,#4449,.F.);
#5638=ORIENTED_EDGE('',*,*,#4451,.F.);
#5639=ORIENTED_EDGE('',*,*,#4452,.T.);
#5640=ORIENTED_EDGE('',*,*,#4453,.T.);
#5641=ORIENTED_EDGE('',*,*,#4452,.F.);
#5642=ORIENTED_EDGE('',*,*,#4451,.T.);
#5643=ORIENTED_EDGE('',*,*,#4448,.T.);
#5644=ORIENTED_EDGE('',*,*,#4453,.F.);
#5645=ORIENTED_EDGE('',*,*,#4450,.F.);
#5646=ORIENTED_EDGE('',*,*,#4454,.F.);
#5647=ORIENTED_EDGE('',*,*,#4455,.T.);
#5648=ORIENTED_EDGE('',*,*,#4456,.F.);
#5649=ORIENTED_EDGE('',*,*,#4455,.F.);
#5650=ORIENTED_EDGE('',*,*,#4457,.F.);
#5651=ORIENTED_EDGE('',*,*,#4458,.T.);
#5652=ORIENTED_EDGE('',*,*,#4459,.F.);
#5653=ORIENTED_EDGE('',*,*,#4458,.F.);
#5654=ORIENTED_EDGE('',*,*,#4460,.F.);
#5655=ORIENTED_EDGE('',*,*,#4461,.T.);
#5656=ORIENTED_EDGE('',*,*,#4462,.F.);
#5657=ORIENTED_EDGE('',*,*,#4461,.F.);
#5658=ORIENTED_EDGE('',*,*,#4463,.F.);
#5659=ORIENTED_EDGE('',*,*,#4464,.T.);
#5660=ORIENTED_EDGE('',*,*,#4465,.F.);
#5661=ORIENTED_EDGE('',*,*,#4464,.F.);
#5662=ORIENTED_EDGE('',*,*,#4466,.F.);
#5663=ORIENTED_EDGE('',*,*,#4467,.T.);
#5664=ORIENTED_EDGE('',*,*,#4468,.T.);
#5665=ORIENTED_EDGE('',*,*,#4467,.F.);
#5666=ORIENTED_EDGE('',*,*,#4469,.F.);
#5667=ORIENTED_EDGE('',*,*,#4470,.T.);
#5668=ORIENTED_EDGE('',*,*,#4471,.T.);
#5669=ORIENTED_EDGE('',*,*,#4470,.F.);
#5670=ORIENTED_EDGE('',*,*,#4469,.T.);
#5671=ORIENTED_EDGE('',*,*,#4466,.T.);
#5672=ORIENTED_EDGE('',*,*,#4465,.T.);
#5673=ORIENTED_EDGE('',*,*,#4462,.T.);
#5674=ORIENTED_EDGE('',*,*,#4459,.T.);
#5675=ORIENTED_EDGE('',*,*,#4456,.T.);
#5676=ORIENTED_EDGE('',*,*,#4471,.F.);
#5677=ORIENTED_EDGE('',*,*,#4468,.F.);
#5678=ORIENTED_EDGE('',*,*,#4463,.T.);
#5679=ORIENTED_EDGE('',*,*,#4460,.T.);
#5680=ORIENTED_EDGE('',*,*,#4457,.T.);
#5681=ORIENTED_EDGE('',*,*,#4454,.T.);
#5682=ORIENTED_EDGE('',*,*,#4472,.F.);
#5683=ORIENTED_EDGE('',*,*,#4473,.T.);
#5684=ORIENTED_EDGE('',*,*,#4474,.F.);
#5685=ORIENTED_EDGE('',*,*,#4473,.F.);
#5686=ORIENTED_EDGE('',*,*,#4475,.F.);
#5687=ORIENTED_EDGE('',*,*,#4476,.T.);
#5688=ORIENTED_EDGE('',*,*,#4477,.F.);
#5689=ORIENTED_EDGE('',*,*,#4476,.F.);
#5690=ORIENTED_EDGE('',*,*,#4478,.F.);
#5691=ORIENTED_EDGE('',*,*,#4479,.T.);
#5692=ORIENTED_EDGE('',*,*,#4480,.F.);
#5693=ORIENTED_EDGE('',*,*,#4479,.F.);
#5694=ORIENTED_EDGE('',*,*,#4481,.F.);
#5695=ORIENTED_EDGE('',*,*,#4482,.T.);
#5696=ORIENTED_EDGE('',*,*,#4483,.F.);
#5697=ORIENTED_EDGE('',*,*,#4482,.F.);
#5698=ORIENTED_EDGE('',*,*,#4484,.F.);
#5699=ORIENTED_EDGE('',*,*,#4485,.T.);
#5700=ORIENTED_EDGE('',*,*,#4486,.T.);
#5701=ORIENTED_EDGE('',*,*,#4485,.F.);
#5702=ORIENTED_EDGE('',*,*,#4487,.F.);
#5703=ORIENTED_EDGE('',*,*,#4488,.T.);
#5704=ORIENTED_EDGE('',*,*,#4489,.T.);
#5705=ORIENTED_EDGE('',*,*,#4488,.F.);
#5706=ORIENTED_EDGE('',*,*,#4487,.T.);
#5707=ORIENTED_EDGE('',*,*,#4484,.T.);
#5708=ORIENTED_EDGE('',*,*,#4483,.T.);
#5709=ORIENTED_EDGE('',*,*,#4480,.T.);
#5710=ORIENTED_EDGE('',*,*,#4477,.T.);
#5711=ORIENTED_EDGE('',*,*,#4474,.T.);
#5712=ORIENTED_EDGE('',*,*,#4489,.F.);
#5713=ORIENTED_EDGE('',*,*,#4486,.F.);
#5714=ORIENTED_EDGE('',*,*,#4481,.T.);
#5715=ORIENTED_EDGE('',*,*,#4478,.T.);
#5716=ORIENTED_EDGE('',*,*,#4475,.T.);
#5717=ORIENTED_EDGE('',*,*,#4472,.T.);
#5718=ORIENTED_EDGE('',*,*,#4490,.F.);
#5719=ORIENTED_EDGE('',*,*,#4491,.T.);
#5720=ORIENTED_EDGE('',*,*,#4492,.T.);
#5721=ORIENTED_EDGE('',*,*,#4491,.F.);
#5722=ORIENTED_EDGE('',*,*,#4493,.F.);
#5723=ORIENTED_EDGE('',*,*,#4494,.T.);
#5724=ORIENTED_EDGE('',*,*,#4495,.T.);
#5725=ORIENTED_EDGE('',*,*,#4494,.F.);
#5726=ORIENTED_EDGE('',*,*,#4493,.T.);
#5727=ORIENTED_EDGE('',*,*,#4490,.T.);
#5728=ORIENTED_EDGE('',*,*,#4495,.F.);
#5729=ORIENTED_EDGE('',*,*,#4492,.F.);
#5730=ORIENTED_EDGE('',*,*,#4496,.F.);
#5731=ORIENTED_EDGE('',*,*,#4497,.T.);
#5732=ORIENTED_EDGE('',*,*,#4498,.F.);
#5733=ORIENTED_EDGE('',*,*,#4497,.F.);
#5734=ORIENTED_EDGE('',*,*,#4499,.F.);
#5735=ORIENTED_EDGE('',*,*,#4500,.T.);
#5736=ORIENTED_EDGE('',*,*,#4501,.F.);
#5737=ORIENTED_EDGE('',*,*,#4500,.F.);
#5738=ORIENTED_EDGE('',*,*,#4502,.F.);
#5739=ORIENTED_EDGE('',*,*,#4503,.T.);
#5740=ORIENTED_EDGE('',*,*,#4504,.F.);
#5741=ORIENTED_EDGE('',*,*,#4503,.F.);
#5742=ORIENTED_EDGE('',*,*,#4505,.F.);
#5743=ORIENTED_EDGE('',*,*,#4506,.T.);
#5744=ORIENTED_EDGE('',*,*,#4507,.F.);
#5745=ORIENTED_EDGE('',*,*,#4506,.F.);
#5746=ORIENTED_EDGE('',*,*,#4508,.F.);
#5747=ORIENTED_EDGE('',*,*,#4509,.T.);
#5748=ORIENTED_EDGE('',*,*,#4510,.T.);
#5749=ORIENTED_EDGE('',*,*,#4509,.F.);
#5750=ORIENTED_EDGE('',*,*,#4511,.F.);
#5751=ORIENTED_EDGE('',*,*,#4512,.T.);
#5752=ORIENTED_EDGE('',*,*,#4513,.T.);
#5753=ORIENTED_EDGE('',*,*,#4512,.F.);
#5754=ORIENTED_EDGE('',*,*,#4511,.T.);
#5755=ORIENTED_EDGE('',*,*,#4508,.T.);
#5756=ORIENTED_EDGE('',*,*,#4507,.T.);
#5757=ORIENTED_EDGE('',*,*,#4504,.T.);
#5758=ORIENTED_EDGE('',*,*,#4501,.T.);
#5759=ORIENTED_EDGE('',*,*,#4498,.T.);
#5760=ORIENTED_EDGE('',*,*,#4513,.F.);
#5761=ORIENTED_EDGE('',*,*,#4510,.F.);
#5762=ORIENTED_EDGE('',*,*,#4505,.T.);
#5763=ORIENTED_EDGE('',*,*,#4502,.T.);
#5764=ORIENTED_EDGE('',*,*,#4499,.T.);
#5765=ORIENTED_EDGE('',*,*,#4496,.T.);
#5766=ORIENTED_EDGE('',*,*,#4514,.F.);
#5767=ORIENTED_EDGE('',*,*,#4515,.T.);
#5768=ORIENTED_EDGE('',*,*,#4516,.F.);
#5769=ORIENTED_EDGE('',*,*,#4515,.F.);
#5770=ORIENTED_EDGE('',*,*,#4517,.F.);
#5771=ORIENTED_EDGE('',*,*,#4518,.T.);
#5772=ORIENTED_EDGE('',*,*,#4519,.F.);
#5773=ORIENTED_EDGE('',*,*,#4518,.F.);
#5774=ORIENTED_EDGE('',*,*,#4520,.F.);
#5775=ORIENTED_EDGE('',*,*,#4521,.T.);
#5776=ORIENTED_EDGE('',*,*,#4522,.F.);
#5777=ORIENTED_EDGE('',*,*,#4521,.F.);
#5778=ORIENTED_EDGE('',*,*,#4523,.F.);
#5779=ORIENTED_EDGE('',*,*,#4524,.T.);
#5780=ORIENTED_EDGE('',*,*,#4525,.F.);
#5781=ORIENTED_EDGE('',*,*,#4524,.F.);
#5782=ORIENTED_EDGE('',*,*,#4526,.F.);
#5783=ORIENTED_EDGE('',*,*,#4527,.T.);
#5784=ORIENTED_EDGE('',*,*,#4528,.T.);
#5785=ORIENTED_EDGE('',*,*,#4527,.F.);
#5786=ORIENTED_EDGE('',*,*,#4529,.F.);
#5787=ORIENTED_EDGE('',*,*,#4530,.T.);
#5788=ORIENTED_EDGE('',*,*,#4531,.T.);
#5789=ORIENTED_EDGE('',*,*,#4530,.F.);
#5790=ORIENTED_EDGE('',*,*,#4529,.T.);
#5791=ORIENTED_EDGE('',*,*,#4526,.T.);
#5792=ORIENTED_EDGE('',*,*,#4525,.T.);
#5793=ORIENTED_EDGE('',*,*,#4522,.T.);
#5794=ORIENTED_EDGE('',*,*,#4519,.T.);
#5795=ORIENTED_EDGE('',*,*,#4516,.T.);
#5796=ORIENTED_EDGE('',*,*,#4531,.F.);
#5797=ORIENTED_EDGE('',*,*,#4528,.F.);
#5798=ORIENTED_EDGE('',*,*,#4523,.T.);
#5799=ORIENTED_EDGE('',*,*,#4520,.T.);
#5800=ORIENTED_EDGE('',*,*,#4517,.T.);
#5801=ORIENTED_EDGE('',*,*,#4514,.T.);
#5802=ORIENTED_EDGE('',*,*,#4532,.F.);
#5803=ORIENTED_EDGE('',*,*,#4533,.T.);
#5804=ORIENTED_EDGE('',*,*,#4534,.F.);
#5805=ORIENTED_EDGE('',*,*,#4533,.F.);
#5806=ORIENTED_EDGE('',*,*,#4535,.T.);
#5807=ORIENTED_EDGE('',*,*,#4536,.T.);
#5808=ORIENTED_EDGE('',*,*,#4537,.F.);
#5809=ORIENTED_EDGE('',*,*,#4538,.F.);
#5810=ORIENTED_EDGE('',*,*,#4539,.T.);
#5811=ORIENTED_EDGE('',*,*,#4538,.T.);
#5812=ORIENTED_EDGE('',*,*,#4540,.F.);
#5813=ORIENTED_EDGE('',*,*,#4541,.F.);
#5814=ORIENTED_EDGE('',*,*,#4534,.T.);
#5815=ORIENTED_EDGE('',*,*,#4542,.T.);
#5816=ORIENTED_EDGE('',*,*,#4541,.T.);
#5817=ORIENTED_EDGE('',*,*,#4543,.F.);
#5818=ORIENTED_EDGE('',*,*,#4544,.F.);
#5819=ORIENTED_EDGE('',*,*,#4545,.T.);
#5820=ORIENTED_EDGE('',*,*,#4544,.T.);
#5821=ORIENTED_EDGE('',*,*,#4546,.F.);
#5822=ORIENTED_EDGE('',*,*,#4536,.F.);
#5823=ORIENTED_EDGE('',*,*,#4532,.T.);
#5824=ORIENTED_EDGE('',*,*,#4546,.T.);
#5825=ORIENTED_EDGE('',*,*,#4543,.T.);
#5826=ORIENTED_EDGE('',*,*,#4540,.T.);
#5827=ORIENTED_EDGE('',*,*,#4537,.T.);
#5828=ORIENTED_EDGE('',*,*,#4545,.F.);
#5829=ORIENTED_EDGE('',*,*,#4535,.F.);
#5830=ORIENTED_EDGE('',*,*,#4539,.F.);
#5831=ORIENTED_EDGE('',*,*,#4542,.F.);
#5832=ORIENTED_EDGE('',*,*,#4547,.F.);
#5833=ORIENTED_EDGE('',*,*,#4548,.T.);
#5834=ORIENTED_EDGE('',*,*,#4549,.F.);
#5835=ORIENTED_EDGE('',*,*,#4548,.F.);
#5836=ORIENTED_EDGE('',*,*,#4550,.F.);
#5837=ORIENTED_EDGE('',*,*,#4551,.T.);
#5838=ORIENTED_EDGE('',*,*,#4552,.F.);
#5839=ORIENTED_EDGE('',*,*,#4551,.F.);
#5840=ORIENTED_EDGE('',*,*,#4553,.F.);
#5841=ORIENTED_EDGE('',*,*,#4554,.T.);
#5842=ORIENTED_EDGE('',*,*,#4555,.F.);
#5843=ORIENTED_EDGE('',*,*,#4554,.F.);
#5844=ORIENTED_EDGE('',*,*,#4556,.F.);
#5845=ORIENTED_EDGE('',*,*,#4557,.T.);
#5846=ORIENTED_EDGE('',*,*,#4558,.F.);
#5847=ORIENTED_EDGE('',*,*,#4557,.F.);
#5848=ORIENTED_EDGE('',*,*,#4559,.F.);
#5849=ORIENTED_EDGE('',*,*,#4560,.T.);
#5850=ORIENTED_EDGE('',*,*,#4561,.F.);
#5851=ORIENTED_EDGE('',*,*,#4560,.F.);
#5852=ORIENTED_EDGE('',*,*,#4562,.F.);
#5853=ORIENTED_EDGE('',*,*,#4563,.T.);
#5854=ORIENTED_EDGE('',*,*,#4564,.F.);
#5855=ORIENTED_EDGE('',*,*,#4563,.F.);
#5856=ORIENTED_EDGE('',*,*,#4565,.F.);
#5857=ORIENTED_EDGE('',*,*,#4566,.T.);
#5858=ORIENTED_EDGE('',*,*,#4567,.F.);
#5859=ORIENTED_EDGE('',*,*,#4566,.F.);
#5860=ORIENTED_EDGE('',*,*,#4568,.F.);
#5861=ORIENTED_EDGE('',*,*,#4569,.T.);
#5862=ORIENTED_EDGE('',*,*,#4570,.F.);
#5863=ORIENTED_EDGE('',*,*,#4569,.F.);
#5864=ORIENTED_EDGE('',*,*,#4571,.F.);
#5865=ORIENTED_EDGE('',*,*,#4572,.T.);
#5866=ORIENTED_EDGE('',*,*,#4573,.F.);
#5867=ORIENTED_EDGE('',*,*,#4572,.F.);
#5868=ORIENTED_EDGE('',*,*,#4574,.F.);
#5869=ORIENTED_EDGE('',*,*,#4575,.T.);
#5870=ORIENTED_EDGE('',*,*,#4576,.F.);
#5871=ORIENTED_EDGE('',*,*,#4575,.F.);
#5872=ORIENTED_EDGE('',*,*,#4577,.F.);
#5873=ORIENTED_EDGE('',*,*,#4578,.F.);
#5874=ORIENTED_EDGE('',*,*,#4579,.F.);
#5875=ORIENTED_EDGE('',*,*,#4580,.T.);
#5876=ORIENTED_EDGE('',*,*,#4577,.T.);
#5877=ORIENTED_EDGE('',*,*,#4581,.F.);
#5878=ORIENTED_EDGE('',*,*,#4582,.F.);
#5879=ORIENTED_EDGE('',*,*,#4583,.F.);
#5880=ORIENTED_EDGE('',*,*,#4580,.F.);
#5881=ORIENTED_EDGE('',*,*,#4584,.T.);
#5882=ORIENTED_EDGE('',*,*,#4585,.F.);
#5883=ORIENTED_EDGE('',*,*,#4581,.T.);
#5884=ORIENTED_EDGE('',*,*,#4559,.T.);
#5885=ORIENTED_EDGE('',*,*,#4562,.T.);
#5886=ORIENTED_EDGE('',*,*,#4565,.T.);
#5887=ORIENTED_EDGE('',*,*,#4568,.T.);
#5888=ORIENTED_EDGE('',*,*,#4571,.T.);
#5889=ORIENTED_EDGE('',*,*,#4574,.T.);
#5890=ORIENTED_EDGE('',*,*,#4556,.T.);
#5891=ORIENTED_EDGE('',*,*,#4553,.T.);
#5892=ORIENTED_EDGE('',*,*,#4550,.T.);
#5893=ORIENTED_EDGE('',*,*,#4547,.T.);
#5894=ORIENTED_EDGE('',*,*,#4579,.T.);
#5895=ORIENTED_EDGE('',*,*,#4586,.F.);
#5896=ORIENTED_EDGE('',*,*,#4587,.F.);
#5897=ORIENTED_EDGE('',*,*,#4584,.F.);
#5898=ORIENTED_EDGE('',*,*,#4582,.T.);
#5899=ORIENTED_EDGE('',*,*,#4585,.T.);
#5900=ORIENTED_EDGE('',*,*,#4587,.T.);
#5901=ORIENTED_EDGE('',*,*,#4588,.F.);
#5902=ORIENTED_EDGE('',*,*,#4583,.T.);
#5903=ORIENTED_EDGE('',*,*,#4588,.T.);
#5904=ORIENTED_EDGE('',*,*,#4586,.T.);
#5905=ORIENTED_EDGE('',*,*,#4578,.T.);
#5906=ORIENTED_EDGE('',*,*,#4561,.T.);
#5907=ORIENTED_EDGE('',*,*,#4564,.T.);
#5908=ORIENTED_EDGE('',*,*,#4567,.T.);
#5909=ORIENTED_EDGE('',*,*,#4570,.T.);
#5910=ORIENTED_EDGE('',*,*,#4573,.T.);
#5911=ORIENTED_EDGE('',*,*,#4576,.T.);
#5912=ORIENTED_EDGE('',*,*,#4558,.T.);
#5913=ORIENTED_EDGE('',*,*,#4555,.T.);
#5914=ORIENTED_EDGE('',*,*,#4552,.T.);
#5915=ORIENTED_EDGE('',*,*,#4549,.T.);
#5916=ORIENTED_EDGE('',*,*,#4589,.F.);
#5917=ORIENTED_EDGE('',*,*,#4590,.T.);
#5918=ORIENTED_EDGE('',*,*,#4591,.T.);
#5919=ORIENTED_EDGE('',*,*,#4590,.F.);
#5920=ORIENTED_EDGE('',*,*,#4592,.F.);
#5921=ORIENTED_EDGE('',*,*,#4593,.T.);
#5922=ORIENTED_EDGE('',*,*,#4594,.T.);
#5923=ORIENTED_EDGE('',*,*,#4593,.F.);
#5924=ORIENTED_EDGE('',*,*,#4592,.T.);
#5925=ORIENTED_EDGE('',*,*,#4589,.T.);
#5926=ORIENTED_EDGE('',*,*,#4594,.F.);
#5927=ORIENTED_EDGE('',*,*,#4591,.F.);
#5928=ORIENTED_EDGE('',*,*,#4595,.F.);
#5929=ORIENTED_EDGE('',*,*,#4596,.T.);
#5930=ORIENTED_EDGE('',*,*,#4597,.F.);
#5931=ORIENTED_EDGE('',*,*,#4596,.F.);
#5932=ORIENTED_EDGE('',*,*,#4598,.F.);
#5933=ORIENTED_EDGE('',*,*,#4599,.T.);
#5934=ORIENTED_EDGE('',*,*,#4600,.F.);
#5935=ORIENTED_EDGE('',*,*,#4599,.F.);
#5936=ORIENTED_EDGE('',*,*,#4601,.F.);
#5937=ORIENTED_EDGE('',*,*,#4602,.T.);
#5938=ORIENTED_EDGE('',*,*,#4603,.F.);
#5939=ORIENTED_EDGE('',*,*,#4602,.F.);
#5940=ORIENTED_EDGE('',*,*,#4604,.F.);
#5941=ORIENTED_EDGE('',*,*,#4605,.T.);
#5942=ORIENTED_EDGE('',*,*,#4606,.F.);
#5943=ORIENTED_EDGE('',*,*,#4605,.F.);
#5944=ORIENTED_EDGE('',*,*,#4607,.F.);
#5945=ORIENTED_EDGE('',*,*,#4608,.T.);
#5946=ORIENTED_EDGE('',*,*,#4609,.T.);
#5947=ORIENTED_EDGE('',*,*,#4608,.F.);
#5948=ORIENTED_EDGE('',*,*,#4610,.F.);
#5949=ORIENTED_EDGE('',*,*,#4611,.T.);
#5950=ORIENTED_EDGE('',*,*,#4612,.T.);
#5951=ORIENTED_EDGE('',*,*,#4611,.F.);
#5952=ORIENTED_EDGE('',*,*,#4610,.T.);
#5953=ORIENTED_EDGE('',*,*,#4607,.T.);
#5954=ORIENTED_EDGE('',*,*,#4606,.T.);
#5955=ORIENTED_EDGE('',*,*,#4603,.T.);
#5956=ORIENTED_EDGE('',*,*,#4600,.T.);
#5957=ORIENTED_EDGE('',*,*,#4597,.T.);
#5958=ORIENTED_EDGE('',*,*,#4612,.F.);
#5959=ORIENTED_EDGE('',*,*,#4609,.F.);
#5960=ORIENTED_EDGE('',*,*,#4604,.T.);
#5961=ORIENTED_EDGE('',*,*,#4601,.T.);
#5962=ORIENTED_EDGE('',*,*,#4598,.T.);
#5963=ORIENTED_EDGE('',*,*,#4595,.T.);
#5964=ORIENTED_EDGE('',*,*,#4613,.F.);
#5965=ORIENTED_EDGE('',*,*,#4614,.T.);
#5966=ORIENTED_EDGE('',*,*,#4615,.F.);
#5967=ORIENTED_EDGE('',*,*,#4614,.F.);
#5968=ORIENTED_EDGE('',*,*,#4616,.F.);
#5969=ORIENTED_EDGE('',*,*,#4617,.T.);
#5970=ORIENTED_EDGE('',*,*,#4618,.F.);
#5971=ORIENTED_EDGE('',*,*,#4617,.F.);
#5972=ORIENTED_EDGE('',*,*,#4619,.F.);
#5973=ORIENTED_EDGE('',*,*,#4620,.T.);
#5974=ORIENTED_EDGE('',*,*,#4621,.F.);
#5975=ORIENTED_EDGE('',*,*,#4620,.F.);
#5976=ORIENTED_EDGE('',*,*,#4622,.F.);
#5977=ORIENTED_EDGE('',*,*,#4623,.T.);
#5978=ORIENTED_EDGE('',*,*,#4624,.F.);
#5979=ORIENTED_EDGE('',*,*,#4623,.F.);
#5980=ORIENTED_EDGE('',*,*,#4625,.F.);
#5981=ORIENTED_EDGE('',*,*,#4626,.T.);
#5982=ORIENTED_EDGE('',*,*,#4627,.T.);
#5983=ORIENTED_EDGE('',*,*,#4626,.F.);
#5984=ORIENTED_EDGE('',*,*,#4628,.F.);
#5985=ORIENTED_EDGE('',*,*,#4629,.T.);
#5986=ORIENTED_EDGE('',*,*,#4630,.T.);
#5987=ORIENTED_EDGE('',*,*,#4629,.F.);
#5988=ORIENTED_EDGE('',*,*,#4628,.T.);
#5989=ORIENTED_EDGE('',*,*,#4625,.T.);
#5990=ORIENTED_EDGE('',*,*,#4624,.T.);
#5991=ORIENTED_EDGE('',*,*,#4621,.T.);
#5992=ORIENTED_EDGE('',*,*,#4618,.T.);
#5993=ORIENTED_EDGE('',*,*,#4615,.T.);
#5994=ORIENTED_EDGE('',*,*,#4630,.F.);
#5995=ORIENTED_EDGE('',*,*,#4627,.F.);
#5996=ORIENTED_EDGE('',*,*,#4622,.T.);
#5997=ORIENTED_EDGE('',*,*,#4619,.T.);
#5998=ORIENTED_EDGE('',*,*,#4616,.T.);
#5999=ORIENTED_EDGE('',*,*,#4613,.T.);
#6000=ORIENTED_EDGE('',*,*,#4631,.F.);
#6001=ORIENTED_EDGE('',*,*,#4632,.T.);
#6002=ORIENTED_EDGE('',*,*,#4633,.T.);
#6003=ORIENTED_EDGE('',*,*,#4632,.F.);
#6004=ORIENTED_EDGE('',*,*,#4634,.F.);
#6005=ORIENTED_EDGE('',*,*,#4635,.T.);
#6006=ORIENTED_EDGE('',*,*,#4636,.T.);
#6007=ORIENTED_EDGE('',*,*,#4635,.F.);
#6008=ORIENTED_EDGE('',*,*,#4634,.T.);
#6009=ORIENTED_EDGE('',*,*,#4631,.T.);
#6010=ORIENTED_EDGE('',*,*,#4636,.F.);
#6011=ORIENTED_EDGE('',*,*,#4633,.F.);
#6012=ORIENTED_EDGE('',*,*,#4637,.F.);
#6013=ORIENTED_EDGE('',*,*,#4638,.T.);
#6014=ORIENTED_EDGE('',*,*,#4639,.F.);
#6015=ORIENTED_EDGE('',*,*,#4638,.F.);
#6016=ORIENTED_EDGE('',*,*,#4640,.F.);
#6017=ORIENTED_EDGE('',*,*,#4641,.T.);
#6018=ORIENTED_EDGE('',*,*,#4642,.F.);
#6019=ORIENTED_EDGE('',*,*,#4641,.F.);
#6020=ORIENTED_EDGE('',*,*,#4643,.F.);
#6021=ORIENTED_EDGE('',*,*,#4644,.T.);
#6022=ORIENTED_EDGE('',*,*,#4645,.F.);
#6023=ORIENTED_EDGE('',*,*,#4644,.F.);
#6024=ORIENTED_EDGE('',*,*,#4646,.F.);
#6025=ORIENTED_EDGE('',*,*,#4647,.T.);
#6026=ORIENTED_EDGE('',*,*,#4648,.F.);
#6027=ORIENTED_EDGE('',*,*,#4647,.F.);
#6028=ORIENTED_EDGE('',*,*,#4649,.F.);
#6029=ORIENTED_EDGE('',*,*,#4650,.T.);
#6030=ORIENTED_EDGE('',*,*,#4651,.T.);
#6031=ORIENTED_EDGE('',*,*,#4650,.F.);
#6032=ORIENTED_EDGE('',*,*,#4652,.F.);
#6033=ORIENTED_EDGE('',*,*,#4653,.T.);
#6034=ORIENTED_EDGE('',*,*,#4654,.T.);
#6035=ORIENTED_EDGE('',*,*,#4653,.F.);
#6036=ORIENTED_EDGE('',*,*,#4652,.T.);
#6037=ORIENTED_EDGE('',*,*,#4649,.T.);
#6038=ORIENTED_EDGE('',*,*,#4648,.T.);
#6039=ORIENTED_EDGE('',*,*,#4645,.T.);
#6040=ORIENTED_EDGE('',*,*,#4642,.T.);
#6041=ORIENTED_EDGE('',*,*,#4639,.T.);
#6042=ORIENTED_EDGE('',*,*,#4654,.F.);
#6043=ORIENTED_EDGE('',*,*,#4651,.F.);
#6044=ORIENTED_EDGE('',*,*,#4646,.T.);
#6045=ORIENTED_EDGE('',*,*,#4643,.T.);
#6046=ORIENTED_EDGE('',*,*,#4640,.T.);
#6047=ORIENTED_EDGE('',*,*,#4637,.T.);
#6048=ORIENTED_EDGE('',*,*,#4655,.F.);
#6049=ORIENTED_EDGE('',*,*,#4656,.T.);
#6050=ORIENTED_EDGE('',*,*,#4657,.F.);
#6051=ORIENTED_EDGE('',*,*,#4656,.F.);
#6052=ORIENTED_EDGE('',*,*,#4658,.F.);
#6053=ORIENTED_EDGE('',*,*,#4659,.T.);
#6054=ORIENTED_EDGE('',*,*,#4660,.F.);
#6055=ORIENTED_EDGE('',*,*,#4659,.F.);
#6056=ORIENTED_EDGE('',*,*,#4661,.F.);
#6057=ORIENTED_EDGE('',*,*,#4662,.T.);
#6058=ORIENTED_EDGE('',*,*,#4663,.F.);
#6059=ORIENTED_EDGE('',*,*,#4662,.F.);
#6060=ORIENTED_EDGE('',*,*,#4664,.F.);
#6061=ORIENTED_EDGE('',*,*,#4665,.T.);
#6062=ORIENTED_EDGE('',*,*,#4666,.F.);
#6063=ORIENTED_EDGE('',*,*,#4665,.F.);
#6064=ORIENTED_EDGE('',*,*,#4667,.F.);
#6065=ORIENTED_EDGE('',*,*,#4668,.T.);
#6066=ORIENTED_EDGE('',*,*,#4669,.T.);
#6067=ORIENTED_EDGE('',*,*,#4668,.F.);
#6068=ORIENTED_EDGE('',*,*,#4670,.F.);
#6069=ORIENTED_EDGE('',*,*,#4671,.T.);
#6070=ORIENTED_EDGE('',*,*,#4672,.T.);
#6071=ORIENTED_EDGE('',*,*,#4671,.F.);
#6072=ORIENTED_EDGE('',*,*,#4670,.T.);
#6073=ORIENTED_EDGE('',*,*,#4667,.T.);
#6074=ORIENTED_EDGE('',*,*,#4666,.T.);
#6075=ORIENTED_EDGE('',*,*,#4663,.T.);
#6076=ORIENTED_EDGE('',*,*,#4660,.T.);
#6077=ORIENTED_EDGE('',*,*,#4657,.T.);
#6078=ORIENTED_EDGE('',*,*,#4672,.F.);
#6079=ORIENTED_EDGE('',*,*,#4669,.F.);
#6080=ORIENTED_EDGE('',*,*,#4664,.T.);
#6081=ORIENTED_EDGE('',*,*,#4661,.T.);
#6082=ORIENTED_EDGE('',*,*,#4658,.T.);
#6083=ORIENTED_EDGE('',*,*,#4655,.T.);
#6084=ORIENTED_EDGE('',*,*,#4673,.F.);
#6085=ORIENTED_EDGE('',*,*,#4674,.F.);
#6086=ORIENTED_EDGE('',*,*,#4675,.T.);
#6087=ORIENTED_EDGE('',*,*,#4676,.F.);
#6088=ORIENTED_EDGE('',*,*,#4677,.F.);
#6089=ORIENTED_EDGE('',*,*,#4675,.F.);
#6090=ORIENTED_EDGE('',*,*,#4676,.T.);
#6091=ORIENTED_EDGE('',*,*,#4677,.T.);
#6092=ORIENTED_EDGE('',*,*,#4678,.T.);
#6093=ORIENTED_EDGE('',*,*,#4679,.T.);
#6094=ORIENTED_EDGE('',*,*,#4678,.F.);
#6095=ORIENTED_EDGE('',*,*,#4680,.T.);
#6096=ORIENTED_EDGE('',*,*,#4681,.T.);
#6097=ORIENTED_EDGE('',*,*,#4682,.F.);
#6098=ORIENTED_EDGE('',*,*,#4681,.F.);
#6099=ORIENTED_EDGE('',*,*,#4682,.T.);
#6100=ORIENTED_EDGE('',*,*,#4683,.T.);
#6101=ORIENTED_EDGE('',*,*,#4684,.F.);
#6102=ORIENTED_EDGE('',*,*,#4683,.F.);
#6103=ORIENTED_EDGE('',*,*,#4679,.F.);
#6104=ORIENTED_EDGE('',*,*,#4684,.T.);
#6105=ORIENTED_EDGE('',*,*,#4685,.F.);
#6106=ORIENTED_EDGE('',*,*,#4686,.T.);
#6107=ORIENTED_EDGE('',*,*,#4673,.T.);
#6108=ORIENTED_EDGE('',*,*,#4674,.T.);
#6109=ORIENTED_EDGE('',*,*,#4686,.F.);
#6110=ORIENTED_EDGE('',*,*,#4685,.T.);
#6111=ORIENTED_EDGE('',*,*,#4687,.F.);
#6112=ORIENTED_EDGE('',*,*,#4687,.T.);
#6113=ORIENTED_EDGE('',*,*,#4688,.T.);
#6114=ORIENTED_EDGE('',*,*,#4680,.F.);
#6115=ORIENTED_EDGE('',*,*,#4688,.F.);
#6116=ORIENTED_EDGE('',*,*,#4689,.F.);
#6117=ORIENTED_EDGE('',*,*,#4690,.F.);
#6118=ORIENTED_EDGE('',*,*,#4691,.T.);
#6119=ORIENTED_EDGE('',*,*,#4692,.F.);
#6120=ORIENTED_EDGE('',*,*,#4693,.F.);
#6121=ORIENTED_EDGE('',*,*,#4691,.F.);
#6122=ORIENTED_EDGE('',*,*,#4694,.T.);
#6123=ORIENTED_EDGE('',*,*,#4695,.T.);
#6124=ORIENTED_EDGE('',*,*,#4692,.T.);
#6125=ORIENTED_EDGE('',*,*,#4693,.T.);
#6126=ORIENTED_EDGE('',*,*,#4695,.F.);
#6127=ORIENTED_EDGE('',*,*,#4696,.F.);
#6128=ORIENTED_EDGE('',*,*,#4697,.T.);
#6129=ORIENTED_EDGE('',*,*,#4698,.F.);
#6130=ORIENTED_EDGE('',*,*,#4699,.T.);
#6131=ORIENTED_EDGE('',*,*,#4696,.T.);
#6132=ORIENTED_EDGE('',*,*,#4699,.F.);
#6133=ORIENTED_EDGE('',*,*,#4700,.F.);
#6134=ORIENTED_EDGE('',*,*,#4701,.T.);
#6135=ORIENTED_EDGE('',*,*,#4698,.T.);
#6136=ORIENTED_EDGE('',*,*,#4701,.F.);
#6137=ORIENTED_EDGE('',*,*,#4702,.F.);
#6138=ORIENTED_EDGE('',*,*,#4703,.T.);
#6139=ORIENTED_EDGE('',*,*,#4700,.T.);
#6140=ORIENTED_EDGE('',*,*,#4703,.F.);
#6141=ORIENTED_EDGE('',*,*,#4702,.T.);
#6142=ORIENTED_EDGE('',*,*,#4694,.F.);
#6143=ORIENTED_EDGE('',*,*,#4689,.T.);
#6144=ORIENTED_EDGE('',*,*,#4690,.T.);
#6145=ORIENTED_EDGE('',*,*,#4704,.T.);
#6146=ORIENTED_EDGE('',*,*,#4697,.F.);
#6147=ORIENTED_EDGE('',*,*,#4704,.F.);
#6148=ORIENTED_EDGE('',*,*,#4705,.T.);
#6149=ORIENTED_EDGE('',*,*,#4705,.F.);
#6150=ORIENTED_EDGE('',*,*,#4706,.T.);
#6151=ORIENTED_EDGE('',*,*,#4706,.F.);
#6152=ORIENTED_EDGE('',*,*,#4707,.T.);
#6153=ORIENTED_EDGE('',*,*,#4707,.F.);
#6154=ORIENTED_EDGE('',*,*,#4708,.T.);
#6155=ORIENTED_EDGE('',*,*,#4708,.F.);
#6156=ORIENTED_EDGE('',*,*,#4709,.T.);
#6157=ORIENTED_EDGE('',*,*,#4709,.F.);
#6158=ORIENTED_EDGE('',*,*,#4710,.T.);
#6159=ORIENTED_EDGE('',*,*,#4710,.F.);
#6160=ORIENTED_EDGE('',*,*,#4711,.T.);
#6161=ORIENTED_EDGE('',*,*,#4711,.F.);
#6162=ORIENTED_EDGE('',*,*,#4712,.T.);
#6163=ORIENTED_EDGE('',*,*,#4712,.F.);
#6164=ORIENTED_EDGE('',*,*,#4713,.F.);
#6165=ORIENTED_EDGE('',*,*,#4714,.F.);
#6166=ORIENTED_EDGE('',*,*,#4715,.F.);
#6167=ORIENTED_EDGE('',*,*,#4716,.F.);
#6168=ORIENTED_EDGE('',*,*,#4715,.T.);
#6169=ORIENTED_EDGE('',*,*,#4717,.F.);
#6170=ORIENTED_EDGE('',*,*,#4718,.T.);
#6171=ORIENTED_EDGE('',*,*,#4719,.F.);
#6172=ORIENTED_EDGE('',*,*,#4720,.T.);
#6173=ORIENTED_EDGE('',*,*,#4721,.F.);
#6174=ORIENTED_EDGE('',*,*,#4722,.T.);
#6175=ORIENTED_EDGE('',*,*,#4723,.T.);
#6176=ORIENTED_EDGE('',*,*,#4724,.F.);
#6177=ORIENTED_EDGE('',*,*,#4723,.F.);
#6178=ORIENTED_EDGE('',*,*,#4725,.T.);
#6179=ORIENTED_EDGE('',*,*,#4726,.F.);
#6180=ORIENTED_EDGE('',*,*,#4727,.T.);
#6181=ORIENTED_EDGE('',*,*,#4728,.F.);
#6182=ORIENTED_EDGE('',*,*,#4729,.T.);
#6183=ORIENTED_EDGE('',*,*,#4730,.F.);
#6184=ORIENTED_EDGE('',*,*,#4731,.T.);
#6185=ORIENTED_EDGE('',*,*,#4732,.F.);
#6186=ORIENTED_EDGE('',*,*,#4733,.T.);
#6187=ORIENTED_EDGE('',*,*,#4734,.F.);
#6188=ORIENTED_EDGE('',*,*,#4714,.T.);
#6189=ORIENTED_EDGE('',*,*,#4735,.T.);
#6190=ORIENTED_EDGE('',*,*,#4736,.T.);
#6191=ORIENTED_EDGE('',*,*,#4717,.T.);
#6192=ORIENTED_EDGE('',*,*,#4737,.F.);
#6193=ORIENTED_EDGE('',*,*,#4738,.F.);
#6194=ORIENTED_EDGE('',*,*,#4718,.F.);
#6195=ORIENTED_EDGE('',*,*,#4736,.F.);
#6196=ORIENTED_EDGE('',*,*,#4738,.T.);
#6197=ORIENTED_EDGE('',*,*,#4739,.T.);
#6198=ORIENTED_EDGE('',*,*,#4740,.T.);
#6199=ORIENTED_EDGE('',*,*,#4719,.T.);
#6200=ORIENTED_EDGE('',*,*,#4741,.F.);
#6201=ORIENTED_EDGE('',*,*,#4742,.F.);
#6202=ORIENTED_EDGE('',*,*,#4720,.F.);
#6203=ORIENTED_EDGE('',*,*,#4740,.F.);
#6204=ORIENTED_EDGE('',*,*,#4742,.T.);
#6205=ORIENTED_EDGE('',*,*,#4743,.T.);
#6206=ORIENTED_EDGE('',*,*,#4744,.T.);
#6207=ORIENTED_EDGE('',*,*,#4721,.T.);
#6208=ORIENTED_EDGE('',*,*,#4745,.F.);
#6209=ORIENTED_EDGE('',*,*,#4746,.F.);
#6210=ORIENTED_EDGE('',*,*,#4725,.F.);
#6211=ORIENTED_EDGE('',*,*,#4722,.F.);
#6212=ORIENTED_EDGE('',*,*,#4744,.F.);
#6213=ORIENTED_EDGE('',*,*,#4747,.F.);
#6214=ORIENTED_EDGE('',*,*,#4746,.T.);
#6215=ORIENTED_EDGE('',*,*,#4748,.T.);
#6216=ORIENTED_EDGE('',*,*,#4749,.T.);
#6217=ORIENTED_EDGE('',*,*,#4726,.T.);
#6218=ORIENTED_EDGE('',*,*,#4750,.F.);
#6219=ORIENTED_EDGE('',*,*,#4751,.F.);
#6220=ORIENTED_EDGE('',*,*,#4727,.F.);
#6221=ORIENTED_EDGE('',*,*,#4749,.F.);
#6222=ORIENTED_EDGE('',*,*,#4751,.T.);
#6223=ORIENTED_EDGE('',*,*,#4752,.T.);
#6224=ORIENTED_EDGE('',*,*,#4753,.T.);
#6225=ORIENTED_EDGE('',*,*,#4728,.T.);
#6226=ORIENTED_EDGE('',*,*,#4754,.F.);
#6227=ORIENTED_EDGE('',*,*,#4755,.F.);
#6228=ORIENTED_EDGE('',*,*,#4729,.F.);
#6229=ORIENTED_EDGE('',*,*,#4753,.F.);
#6230=ORIENTED_EDGE('',*,*,#4755,.T.);
#6231=ORIENTED_EDGE('',*,*,#4756,.T.);
#6232=ORIENTED_EDGE('',*,*,#4757,.T.);
#6233=ORIENTED_EDGE('',*,*,#4730,.T.);
#6234=ORIENTED_EDGE('',*,*,#4731,.F.);
#6235=ORIENTED_EDGE('',*,*,#4757,.F.);
#6236=ORIENTED_EDGE('',*,*,#4758,.F.);
#6237=ORIENTED_EDGE('',*,*,#4759,.F.);
#6238=ORIENTED_EDGE('',*,*,#4760,.F.);
#6239=ORIENTED_EDGE('',*,*,#4761,.T.);
#6240=ORIENTED_EDGE('',*,*,#4747,.T.);
#6241=ORIENTED_EDGE('',*,*,#4743,.F.);
#6242=ORIENTED_EDGE('',*,*,#4741,.T.);
#6243=ORIENTED_EDGE('',*,*,#4739,.F.);
#6244=ORIENTED_EDGE('',*,*,#4737,.T.);
#6245=ORIENTED_EDGE('',*,*,#4735,.F.);
#6246=ORIENTED_EDGE('',*,*,#4713,.T.);
#6247=ORIENTED_EDGE('',*,*,#4762,.F.);
#6248=ORIENTED_EDGE('',*,*,#4763,.T.);
#6249=ORIENTED_EDGE('',*,*,#4764,.F.);
#6250=ORIENTED_EDGE('',*,*,#4758,.T.);
#6251=ORIENTED_EDGE('',*,*,#4756,.F.);
#6252=ORIENTED_EDGE('',*,*,#4754,.T.);
#6253=ORIENTED_EDGE('',*,*,#4752,.F.);
#6254=ORIENTED_EDGE('',*,*,#4750,.T.);
#6255=ORIENTED_EDGE('',*,*,#4748,.F.);
#6256=ORIENTED_EDGE('',*,*,#4745,.T.);
#6257=ORIENTED_EDGE('',*,*,#4761,.F.);
#6258=ORIENTED_EDGE('',*,*,#4716,.T.);
#6259=ORIENTED_EDGE('',*,*,#4734,.T.);
#6260=ORIENTED_EDGE('',*,*,#4765,.T.);
#6261=ORIENTED_EDGE('',*,*,#4762,.T.);
#6262=ORIENTED_EDGE('',*,*,#4733,.F.);
#6263=ORIENTED_EDGE('',*,*,#4766,.F.);
#6264=ORIENTED_EDGE('',*,*,#4763,.F.);
#6265=ORIENTED_EDGE('',*,*,#4765,.F.);
#6266=ORIENTED_EDGE('',*,*,#4724,.T.);
#6267=ORIENTED_EDGE('',*,*,#4760,.T.);
#6268=ORIENTED_EDGE('',*,*,#4759,.T.);
#6269=ORIENTED_EDGE('',*,*,#4764,.T.);
#6270=ORIENTED_EDGE('',*,*,#4766,.T.);
#6271=ORIENTED_EDGE('',*,*,#4732,.T.);
#6272=ORIENTED_EDGE('',*,*,#4767,.F.);
#6273=ORIENTED_EDGE('',*,*,#4768,.T.);
#6274=ORIENTED_EDGE('',*,*,#4769,.F.);
#6275=ORIENTED_EDGE('',*,*,#4770,.T.);
#6276=ORIENTED_EDGE('',*,*,#4767,.T.);
#6277=ORIENTED_EDGE('',*,*,#4770,.F.);
#6278=ORIENTED_EDGE('',*,*,#4769,.T.);
#6279=ORIENTED_EDGE('',*,*,#4771,.F.);
#6280=ORIENTED_EDGE('',*,*,#4771,.T.);
#6281=ORIENTED_EDGE('',*,*,#4772,.T.);
#6282=ORIENTED_EDGE('',*,*,#4768,.F.);
#6283=ORIENTED_EDGE('',*,*,#4772,.F.);
#6284=ORIENTED_EDGE('',*,*,#4773,.F.);
#6285=ORIENTED_EDGE('',*,*,#4774,.T.);
#6286=ORIENTED_EDGE('',*,*,#4775,.F.);
#6287=ORIENTED_EDGE('',*,*,#4776,.T.);
#6288=ORIENTED_EDGE('',*,*,#4773,.T.);
#6289=ORIENTED_EDGE('',*,*,#4776,.F.);
#6290=ORIENTED_EDGE('',*,*,#4775,.T.);
#6291=ORIENTED_EDGE('',*,*,#4777,.F.);
#6292=ORIENTED_EDGE('',*,*,#4777,.T.);
#6293=ORIENTED_EDGE('',*,*,#4778,.T.);
#6294=ORIENTED_EDGE('',*,*,#4774,.F.);
#6295=ORIENTED_EDGE('',*,*,#4778,.F.);
#6296=ORIENTED_EDGE('',*,*,#4779,.T.);
#6297=ORIENTED_EDGE('',*,*,#4780,.T.);
#6298=ORIENTED_EDGE('',*,*,#4781,.T.);
#6299=ORIENTED_EDGE('',*,*,#4782,.F.);
#6300=ORIENTED_EDGE('',*,*,#4783,.T.);
#6301=ORIENTED_EDGE('',*,*,#4784,.T.);
#6302=ORIENTED_EDGE('',*,*,#4785,.T.);
#6303=ORIENTED_EDGE('',*,*,#4780,.F.);
#6304=ORIENTED_EDGE('',*,*,#4786,.T.);
#6305=ORIENTED_EDGE('',*,*,#4787,.T.);
#6306=ORIENTED_EDGE('',*,*,#4788,.T.);
#6307=ORIENTED_EDGE('',*,*,#4784,.F.);
#6308=ORIENTED_EDGE('',*,*,#4789,.T.);
#6309=ORIENTED_EDGE('',*,*,#4790,.T.);
#6310=ORIENTED_EDGE('',*,*,#4791,.T.);
#6311=ORIENTED_EDGE('',*,*,#4787,.F.);
#6312=ORIENTED_EDGE('',*,*,#4792,.T.);
#6313=ORIENTED_EDGE('',*,*,#4793,.T.);
#6314=ORIENTED_EDGE('',*,*,#4794,.T.);
#6315=ORIENTED_EDGE('',*,*,#4790,.F.);
#6316=ORIENTED_EDGE('',*,*,#4795,.T.);
#6317=ORIENTED_EDGE('',*,*,#4782,.T.);
#6318=ORIENTED_EDGE('',*,*,#4796,.T.);
#6319=ORIENTED_EDGE('',*,*,#4793,.F.);
#6320=ORIENTED_EDGE('',*,*,#4795,.F.);
#6321=ORIENTED_EDGE('',*,*,#4792,.F.);
#6322=ORIENTED_EDGE('',*,*,#4789,.F.);
#6323=ORIENTED_EDGE('',*,*,#4786,.F.);
#6324=ORIENTED_EDGE('',*,*,#4783,.F.);
#6325=ORIENTED_EDGE('',*,*,#4779,.F.);
#6326=ORIENTED_EDGE('',*,*,#4796,.F.);
#6327=ORIENTED_EDGE('',*,*,#4781,.F.);
#6328=ORIENTED_EDGE('',*,*,#4785,.F.);
#6329=ORIENTED_EDGE('',*,*,#4788,.F.);
#6330=ORIENTED_EDGE('',*,*,#4791,.F.);
#6331=ORIENTED_EDGE('',*,*,#4794,.F.);
#6332=ORIENTED_EDGE('',*,*,#4797,.F.);
#6333=ORIENTED_EDGE('',*,*,#4798,.F.);
#6334=ORIENTED_EDGE('',*,*,#4799,.F.);
#6335=ORIENTED_EDGE('',*,*,#4800,.T.);
#6336=ORIENTED_EDGE('',*,*,#4798,.T.);
#6337=ORIENTED_EDGE('',*,*,#4800,.F.);
#6338=ORIENTED_EDGE('',*,*,#4801,.F.);
#6339=ORIENTED_EDGE('',*,*,#4802,.T.);
#6340=ORIENTED_EDGE('',*,*,#4799,.T.);
#6341=ORIENTED_EDGE('',*,*,#4802,.F.);
#6342=ORIENTED_EDGE('',*,*,#4803,.F.);
#6343=ORIENTED_EDGE('',*,*,#4804,.T.);
#6344=ORIENTED_EDGE('',*,*,#4801,.T.);
#6345=ORIENTED_EDGE('',*,*,#4804,.F.);
#6346=ORIENTED_EDGE('',*,*,#4803,.T.);
#6347=ORIENTED_EDGE('',*,*,#4805,.F.);
#6348=ORIENTED_EDGE('',*,*,#4806,.F.);
#6349=ORIENTED_EDGE('',*,*,#4807,.T.);
#6350=ORIENTED_EDGE('',*,*,#4805,.T.);
#6351=ORIENTED_EDGE('',*,*,#4807,.F.);
#6352=ORIENTED_EDGE('',*,*,#4797,.T.);
#6353=ORIENTED_EDGE('',*,*,#4808,.T.);
#6354=ORIENTED_EDGE('',*,*,#4806,.T.);
#6355=ORIENTED_EDGE('',*,*,#4808,.F.);
#6356=ORIENTED_EDGE('',*,*,#4809,.F.);
#6357=ORIENTED_EDGE('',*,*,#4810,.T.);
#6358=ORIENTED_EDGE('',*,*,#4811,.F.);
#6359=ORIENTED_EDGE('',*,*,#4810,.F.);
#6360=ORIENTED_EDGE('',*,*,#4812,.F.);
#6361=ORIENTED_EDGE('',*,*,#4813,.T.);
#6362=ORIENTED_EDGE('',*,*,#4814,.F.);
#6363=ORIENTED_EDGE('',*,*,#4813,.F.);
#6364=ORIENTED_EDGE('',*,*,#4815,.F.);
#6365=ORIENTED_EDGE('',*,*,#4816,.T.);
#6366=ORIENTED_EDGE('',*,*,#4817,.F.);
#6367=ORIENTED_EDGE('',*,*,#4816,.F.);
#6368=ORIENTED_EDGE('',*,*,#4818,.F.);
#6369=ORIENTED_EDGE('',*,*,#4819,.T.);
#6370=ORIENTED_EDGE('',*,*,#4820,.F.);
#6371=ORIENTED_EDGE('',*,*,#4819,.F.);
#6372=ORIENTED_EDGE('',*,*,#4821,.F.);
#6373=ORIENTED_EDGE('',*,*,#4822,.T.);
#6374=ORIENTED_EDGE('',*,*,#4823,.F.);
#6375=ORIENTED_EDGE('',*,*,#4822,.F.);
#6376=ORIENTED_EDGE('',*,*,#4824,.F.);
#6377=ORIENTED_EDGE('',*,*,#4825,.T.);
#6378=ORIENTED_EDGE('',*,*,#4826,.F.);
#6379=ORIENTED_EDGE('',*,*,#4825,.F.);
#6380=ORIENTED_EDGE('',*,*,#4827,.F.);
#6381=ORIENTED_EDGE('',*,*,#4828,.T.);
#6382=ORIENTED_EDGE('',*,*,#4829,.F.);
#6383=ORIENTED_EDGE('',*,*,#4828,.F.);
#6384=ORIENTED_EDGE('',*,*,#4830,.F.);
#6385=ORIENTED_EDGE('',*,*,#4831,.T.);
#6386=ORIENTED_EDGE('',*,*,#4832,.F.);
#6387=ORIENTED_EDGE('',*,*,#4831,.F.);
#6388=ORIENTED_EDGE('',*,*,#4833,.F.);
#6389=ORIENTED_EDGE('',*,*,#4834,.T.);
#6390=ORIENTED_EDGE('',*,*,#4835,.F.);
#6391=ORIENTED_EDGE('',*,*,#4834,.F.);
#6392=ORIENTED_EDGE('',*,*,#4836,.F.);
#6393=ORIENTED_EDGE('',*,*,#4837,.T.);
#6394=ORIENTED_EDGE('',*,*,#4838,.F.);
#6395=ORIENTED_EDGE('',*,*,#4837,.F.);
#6396=ORIENTED_EDGE('',*,*,#4839,.F.);
#6397=ORIENTED_EDGE('',*,*,#4840,.T.);
#6398=ORIENTED_EDGE('',*,*,#4841,.F.);
#6399=ORIENTED_EDGE('',*,*,#4840,.F.);
#6400=ORIENTED_EDGE('',*,*,#4842,.F.);
#6401=ORIENTED_EDGE('',*,*,#4843,.T.);
#6402=ORIENTED_EDGE('',*,*,#4844,.F.);
#6403=ORIENTED_EDGE('',*,*,#4843,.F.);
#6404=ORIENTED_EDGE('',*,*,#4845,.T.);
#6405=ORIENTED_EDGE('',*,*,#4846,.T.);
#6406=ORIENTED_EDGE('',*,*,#4847,.F.);
#6407=ORIENTED_EDGE('',*,*,#4848,.F.);
#6408=ORIENTED_EDGE('',*,*,#4849,.T.);
#6409=ORIENTED_EDGE('',*,*,#4848,.T.);
#6410=ORIENTED_EDGE('',*,*,#4850,.F.);
#6411=ORIENTED_EDGE('',*,*,#4851,.F.);
#6412=ORIENTED_EDGE('',*,*,#4852,.T.);
#6413=ORIENTED_EDGE('',*,*,#4853,.T.);
#6414=ORIENTED_EDGE('',*,*,#4850,.T.);
#6415=ORIENTED_EDGE('',*,*,#4847,.T.);
#6416=ORIENTED_EDGE('',*,*,#4835,.T.);
#6417=ORIENTED_EDGE('',*,*,#4838,.T.);
#6418=ORIENTED_EDGE('',*,*,#4841,.T.);
#6419=ORIENTED_EDGE('',*,*,#4844,.T.);
#6420=ORIENTED_EDGE('',*,*,#4854,.T.);
#6421=ORIENTED_EDGE('',*,*,#4855,.F.);
#6422=ORIENTED_EDGE('',*,*,#4845,.F.);
#6423=ORIENTED_EDGE('',*,*,#4849,.F.);
#6424=ORIENTED_EDGE('',*,*,#4856,.F.);
#6425=ORIENTED_EDGE('',*,*,#4857,.T.);
#6426=ORIENTED_EDGE('',*,*,#4833,.T.);
#6427=ORIENTED_EDGE('',*,*,#4836,.T.);
#6428=ORIENTED_EDGE('',*,*,#4839,.T.);
#6429=ORIENTED_EDGE('',*,*,#4842,.T.);
#6430=ORIENTED_EDGE('',*,*,#4858,.T.);
#6431=ORIENTED_EDGE('',*,*,#4859,.T.);
#6432=ORIENTED_EDGE('',*,*,#4854,.F.);
#6433=ORIENTED_EDGE('',*,*,#4860,.F.);
#6434=ORIENTED_EDGE('',*,*,#4832,.T.);
#6435=ORIENTED_EDGE('',*,*,#4829,.T.);
#6436=ORIENTED_EDGE('',*,*,#4826,.T.);
#6437=ORIENTED_EDGE('',*,*,#4823,.T.);
#6438=ORIENTED_EDGE('',*,*,#4820,.T.);
#6439=ORIENTED_EDGE('',*,*,#4817,.T.);
#6440=ORIENTED_EDGE('',*,*,#4814,.T.);
#6441=ORIENTED_EDGE('',*,*,#4811,.T.);
#6442=ORIENTED_EDGE('',*,*,#4861,.T.);
#6443=ORIENTED_EDGE('',*,*,#4860,.T.);
#6444=ORIENTED_EDGE('',*,*,#4857,.F.);
#6445=ORIENTED_EDGE('',*,*,#4862,.F.);
#6446=ORIENTED_EDGE('',*,*,#4863,.T.);
#6447=ORIENTED_EDGE('',*,*,#4862,.T.);
#6448=ORIENTED_EDGE('',*,*,#4856,.T.);
#6449=ORIENTED_EDGE('',*,*,#4851,.T.);
#6450=ORIENTED_EDGE('',*,*,#4853,.F.);
#6451=ORIENTED_EDGE('',*,*,#4864,.F.);
#6452=ORIENTED_EDGE('',*,*,#4830,.T.);
#6453=ORIENTED_EDGE('',*,*,#4827,.T.);
#6454=ORIENTED_EDGE('',*,*,#4824,.T.);
#6455=ORIENTED_EDGE('',*,*,#4821,.T.);
#6456=ORIENTED_EDGE('',*,*,#4818,.T.);
#6457=ORIENTED_EDGE('',*,*,#4815,.T.);
#6458=ORIENTED_EDGE('',*,*,#4812,.T.);
#6459=ORIENTED_EDGE('',*,*,#4809,.T.);
#6460=ORIENTED_EDGE('',*,*,#4865,.T.);
#6461=ORIENTED_EDGE('',*,*,#4864,.T.);
#6462=ORIENTED_EDGE('',*,*,#4852,.F.);
#6463=ORIENTED_EDGE('',*,*,#4846,.F.);
#6464=ORIENTED_EDGE('',*,*,#4855,.T.);
#6465=ORIENTED_EDGE('',*,*,#4859,.F.);
#6466=ORIENTED_EDGE('',*,*,#4865,.F.);
#6467=ORIENTED_EDGE('',*,*,#4858,.F.);
#6468=ORIENTED_EDGE('',*,*,#4861,.F.);
#6469=ORIENTED_EDGE('',*,*,#4863,.F.);
#6470=ORIENTED_EDGE('',*,*,#4866,.F.);
#6471=ORIENTED_EDGE('',*,*,#4867,.T.);
#6472=ORIENTED_EDGE('',*,*,#4868,.T.);
#6473=ORIENTED_EDGE('',*,*,#4867,.F.);
#6474=ORIENTED_EDGE('',*,*,#4868,.F.);
#6475=ORIENTED_EDGE('',*,*,#4869,.F.);
#6476=ORIENTED_EDGE('',*,*,#4870,.T.);
#6477=ORIENTED_EDGE('',*,*,#4871,.F.);
#6478=ORIENTED_EDGE('',*,*,#4870,.F.);
#6479=ORIENTED_EDGE('',*,*,#4872,.F.);
#6480=ORIENTED_EDGE('',*,*,#4873,.T.);
#6481=ORIENTED_EDGE('',*,*,#4874,.F.);
#6482=ORIENTED_EDGE('',*,*,#4873,.F.);
#6483=ORIENTED_EDGE('',*,*,#4875,.F.);
#6484=ORIENTED_EDGE('',*,*,#4876,.T.);
#6485=ORIENTED_EDGE('',*,*,#4877,.F.);
#6486=ORIENTED_EDGE('',*,*,#4876,.F.);
#6487=ORIENTED_EDGE('',*,*,#4878,.T.);
#6488=ORIENTED_EDGE('',*,*,#4871,.T.);
#6489=ORIENTED_EDGE('',*,*,#4874,.T.);
#6490=ORIENTED_EDGE('',*,*,#4877,.T.);
#6491=ORIENTED_EDGE('',*,*,#4879,.F.);
#6492=ORIENTED_EDGE('',*,*,#4880,.F.);
#6493=ORIENTED_EDGE('',*,*,#4869,.T.);
#6494=ORIENTED_EDGE('',*,*,#4872,.T.);
#6495=ORIENTED_EDGE('',*,*,#4875,.T.);
#6496=ORIENTED_EDGE('',*,*,#4881,.F.);
#6497=ORIENTED_EDGE('',*,*,#4878,.F.);
#6498=ORIENTED_EDGE('',*,*,#4882,.T.);
#6499=ORIENTED_EDGE('',*,*,#4880,.T.);
#6500=ORIENTED_EDGE('',*,*,#4882,.F.);
#6501=ORIENTED_EDGE('',*,*,#4881,.T.);
#6502=ORIENTED_EDGE('',*,*,#4883,.T.);
#6503=ORIENTED_EDGE('',*,*,#4884,.T.);
#6504=ORIENTED_EDGE('',*,*,#4883,.F.);
#6505=ORIENTED_EDGE('',*,*,#4885,.F.);
#6506=ORIENTED_EDGE('',*,*,#4886,.T.);
#6507=ORIENTED_EDGE('',*,*,#4879,.T.);
#6508=ORIENTED_EDGE('',*,*,#4886,.F.);
#6509=ORIENTED_EDGE('',*,*,#4885,.T.);
#6510=ORIENTED_EDGE('',*,*,#4884,.F.);
#6511=ORIENTED_EDGE('',*,*,#4866,.T.);
#6512=ORIENTED_EDGE('',*,*,#4887,.F.);
#6513=ORIENTED_EDGE('',*,*,#4888,.T.);
#6514=ORIENTED_EDGE('',*,*,#4889,.T.);
#6515=ORIENTED_EDGE('',*,*,#4888,.F.);
#6516=ORIENTED_EDGE('',*,*,#4890,.F.);
#6517=ORIENTED_EDGE('',*,*,#4891,.T.);
#6518=ORIENTED_EDGE('',*,*,#4892,.T.);
#6519=ORIENTED_EDGE('',*,*,#4891,.F.);
#6520=ORIENTED_EDGE('',*,*,#4890,.T.);
#6521=ORIENTED_EDGE('',*,*,#4887,.T.);
#6522=ORIENTED_EDGE('',*,*,#4892,.F.);
#6523=ORIENTED_EDGE('',*,*,#4889,.F.);
#6524=ORIENTED_EDGE('',*,*,#4893,.F.);
#6525=ORIENTED_EDGE('',*,*,#4894,.T.);
#6526=ORIENTED_EDGE('',*,*,#4895,.T.);
#6527=ORIENTED_EDGE('',*,*,#4894,.F.);
#6528=ORIENTED_EDGE('',*,*,#4896,.F.);
#6529=ORIENTED_EDGE('',*,*,#4897,.T.);
#6530=ORIENTED_EDGE('',*,*,#4898,.T.);
#6531=ORIENTED_EDGE('',*,*,#4897,.F.);
#6532=ORIENTED_EDGE('',*,*,#4896,.T.);
#6533=ORIENTED_EDGE('',*,*,#4893,.T.);
#6534=ORIENTED_EDGE('',*,*,#4898,.F.);
#6535=ORIENTED_EDGE('',*,*,#4895,.F.);
#6536=ORIENTED_EDGE('',*,*,#4899,.F.);
#6537=ORIENTED_EDGE('',*,*,#4900,.T.);
#6538=ORIENTED_EDGE('',*,*,#4901,.T.);
#6539=ORIENTED_EDGE('',*,*,#4900,.F.);
#6540=ORIENTED_EDGE('',*,*,#4902,.F.);
#6541=ORIENTED_EDGE('',*,*,#4903,.T.);
#6542=ORIENTED_EDGE('',*,*,#4904,.T.);
#6543=ORIENTED_EDGE('',*,*,#4903,.F.);
#6544=ORIENTED_EDGE('',*,*,#4902,.T.);
#6545=ORIENTED_EDGE('',*,*,#4899,.T.);
#6546=ORIENTED_EDGE('',*,*,#4904,.F.);
#6547=ORIENTED_EDGE('',*,*,#4901,.F.);
#6548=ORIENTED_EDGE('',*,*,#4905,.F.);
#6549=ORIENTED_EDGE('',*,*,#4906,.T.);
#6550=ORIENTED_EDGE('',*,*,#4907,.T.);
#6551=ORIENTED_EDGE('',*,*,#4906,.F.);
#6552=ORIENTED_EDGE('',*,*,#4908,.F.);
#6553=ORIENTED_EDGE('',*,*,#4909,.T.);
#6554=ORIENTED_EDGE('',*,*,#4910,.T.);
#6555=ORIENTED_EDGE('',*,*,#4909,.F.);
#6556=ORIENTED_EDGE('',*,*,#4908,.T.);
#6557=ORIENTED_EDGE('',*,*,#4905,.T.);
#6558=ORIENTED_EDGE('',*,*,#4910,.F.);
#6559=ORIENTED_EDGE('',*,*,#4907,.F.);
#6560=ORIENTED_EDGE('',*,*,#4911,.F.);
#6561=ORIENTED_EDGE('',*,*,#4912,.T.);
#6562=ORIENTED_EDGE('',*,*,#4913,.T.);
#6563=ORIENTED_EDGE('',*,*,#4912,.F.);
#6564=ORIENTED_EDGE('',*,*,#4913,.F.);
#6565=ORIENTED_EDGE('',*,*,#4914,.F.);
#6566=ORIENTED_EDGE('',*,*,#4915,.T.);
#6567=ORIENTED_EDGE('',*,*,#4916,.F.);
#6568=ORIENTED_EDGE('',*,*,#4915,.F.);
#6569=ORIENTED_EDGE('',*,*,#4917,.F.);
#6570=ORIENTED_EDGE('',*,*,#4918,.T.);
#6571=ORIENTED_EDGE('',*,*,#4919,.F.);
#6572=ORIENTED_EDGE('',*,*,#4918,.F.);
#6573=ORIENTED_EDGE('',*,*,#4920,.F.);
#6574=ORIENTED_EDGE('',*,*,#4921,.T.);
#6575=ORIENTED_EDGE('',*,*,#4922,.F.);
#6576=ORIENTED_EDGE('',*,*,#4921,.F.);
#6577=ORIENTED_EDGE('',*,*,#4923,.T.);
#6578=ORIENTED_EDGE('',*,*,#4916,.T.);
#6579=ORIENTED_EDGE('',*,*,#4919,.T.);
#6580=ORIENTED_EDGE('',*,*,#4922,.T.);
#6581=ORIENTED_EDGE('',*,*,#4924,.F.);
#6582=ORIENTED_EDGE('',*,*,#4925,.F.);
#6583=ORIENTED_EDGE('',*,*,#4914,.T.);
#6584=ORIENTED_EDGE('',*,*,#4917,.T.);
#6585=ORIENTED_EDGE('',*,*,#4920,.T.);
#6586=ORIENTED_EDGE('',*,*,#4926,.F.);
#6587=ORIENTED_EDGE('',*,*,#4923,.F.);
#6588=ORIENTED_EDGE('',*,*,#4927,.T.);
#6589=ORIENTED_EDGE('',*,*,#4925,.T.);
#6590=ORIENTED_EDGE('',*,*,#4927,.F.);
#6591=ORIENTED_EDGE('',*,*,#4926,.T.);
#6592=ORIENTED_EDGE('',*,*,#4928,.T.);
#6593=ORIENTED_EDGE('',*,*,#4929,.T.);
#6594=ORIENTED_EDGE('',*,*,#4928,.F.);
#6595=ORIENTED_EDGE('',*,*,#4930,.F.);
#6596=ORIENTED_EDGE('',*,*,#4931,.T.);
#6597=ORIENTED_EDGE('',*,*,#4924,.T.);
#6598=ORIENTED_EDGE('',*,*,#4931,.F.);
#6599=ORIENTED_EDGE('',*,*,#4930,.T.);
#6600=ORIENTED_EDGE('',*,*,#4929,.F.);
#6601=ORIENTED_EDGE('',*,*,#4911,.T.);
#6602=ORIENTED_EDGE('',*,*,#4932,.F.);
#6603=ORIENTED_EDGE('',*,*,#4933,.T.);
#6604=ORIENTED_EDGE('',*,*,#4934,.T.);
#6605=ORIENTED_EDGE('',*,*,#4933,.F.);
#6606=ORIENTED_EDGE('',*,*,#4935,.F.);
#6607=ORIENTED_EDGE('',*,*,#4936,.T.);
#6608=ORIENTED_EDGE('',*,*,#4937,.T.);
#6609=ORIENTED_EDGE('',*,*,#4936,.F.);
#6610=ORIENTED_EDGE('',*,*,#4935,.T.);
#6611=ORIENTED_EDGE('',*,*,#4932,.T.);
#6612=ORIENTED_EDGE('',*,*,#4937,.F.);
#6613=ORIENTED_EDGE('',*,*,#4934,.F.);
#6614=ORIENTED_EDGE('',*,*,#4938,.F.);
#6615=ORIENTED_EDGE('',*,*,#4939,.T.);
#6616=ORIENTED_EDGE('',*,*,#4940,.T.);
#6617=ORIENTED_EDGE('',*,*,#4939,.F.);
#6618=ORIENTED_EDGE('',*,*,#4941,.F.);
#6619=ORIENTED_EDGE('',*,*,#4942,.T.);
#6620=ORIENTED_EDGE('',*,*,#4943,.T.);
#6621=ORIENTED_EDGE('',*,*,#4942,.F.);
#6622=ORIENTED_EDGE('',*,*,#4941,.T.);
#6623=ORIENTED_EDGE('',*,*,#4938,.T.);
#6624=ORIENTED_EDGE('',*,*,#4943,.F.);
#6625=ORIENTED_EDGE('',*,*,#4940,.F.);
#6626=ORIENTED_EDGE('',*,*,#4944,.F.);
#6627=ORIENTED_EDGE('',*,*,#4945,.T.);
#6628=ORIENTED_EDGE('',*,*,#4946,.T.);
#6629=ORIENTED_EDGE('',*,*,#4945,.F.);
#6630=ORIENTED_EDGE('',*,*,#4947,.F.);
#6631=ORIENTED_EDGE('',*,*,#4948,.T.);
#6632=ORIENTED_EDGE('',*,*,#4949,.T.);
#6633=ORIENTED_EDGE('',*,*,#4948,.F.);
#6634=ORIENTED_EDGE('',*,*,#4947,.T.);
#6635=ORIENTED_EDGE('',*,*,#4944,.T.);
#6636=ORIENTED_EDGE('',*,*,#4949,.F.);
#6637=ORIENTED_EDGE('',*,*,#4946,.F.);
#6638=ORIENTED_EDGE('',*,*,#4950,.F.);
#6639=ORIENTED_EDGE('',*,*,#4951,.T.);
#6640=ORIENTED_EDGE('',*,*,#4952,.T.);
#6641=ORIENTED_EDGE('',*,*,#4951,.F.);
#6642=ORIENTED_EDGE('',*,*,#4953,.F.);
#6643=ORIENTED_EDGE('',*,*,#4954,.T.);
#6644=ORIENTED_EDGE('',*,*,#4955,.T.);
#6645=ORIENTED_EDGE('',*,*,#4954,.F.);
#6646=ORIENTED_EDGE('',*,*,#4953,.T.);
#6647=ORIENTED_EDGE('',*,*,#4950,.T.);
#6648=ORIENTED_EDGE('',*,*,#4955,.F.);
#6649=ORIENTED_EDGE('',*,*,#4952,.F.);
#6650=ORIENTED_EDGE('',*,*,#4956,.F.);
#6651=ORIENTED_EDGE('',*,*,#4957,.F.);
#6652=ORIENTED_EDGE('',*,*,#4958,.T.);
#6653=ORIENTED_EDGE('',*,*,#4956,.T.);
#6654=ORIENTED_EDGE('',*,*,#4958,.F.);
#6655=ORIENTED_EDGE('',*,*,#4959,.F.);
#6656=ORIENTED_EDGE('',*,*,#4960,.T.);
#6657=ORIENTED_EDGE('',*,*,#4957,.T.);
#6658=ORIENTED_EDGE('',*,*,#4960,.F.);
#6659=ORIENTED_EDGE('',*,*,#4961,.F.);
#6660=ORIENTED_EDGE('',*,*,#4962,.T.);
#6661=ORIENTED_EDGE('',*,*,#4959,.T.);
#6662=ORIENTED_EDGE('',*,*,#4962,.F.);
#6663=ORIENTED_EDGE('',*,*,#4961,.T.);
#6664=ORIENTED_EDGE('',*,*,#4963,.F.);
#6665=ORIENTED_EDGE('',*,*,#4964,.F.);
#6666=ORIENTED_EDGE('',*,*,#4965,.T.);
#6667=ORIENTED_EDGE('',*,*,#4963,.T.);
#6668=ORIENTED_EDGE('',*,*,#4965,.F.);
#6669=ORIENTED_EDGE('',*,*,#4966,.F.);
#6670=ORIENTED_EDGE('',*,*,#4967,.T.);
#6671=ORIENTED_EDGE('',*,*,#4964,.T.);
#6672=ORIENTED_EDGE('',*,*,#4967,.F.);
#6673=ORIENTED_EDGE('',*,*,#4968,.F.);
#6674=ORIENTED_EDGE('',*,*,#4969,.T.);
#6675=ORIENTED_EDGE('',*,*,#4966,.T.);
#6676=ORIENTED_EDGE('',*,*,#4969,.F.);
#6677=ORIENTED_EDGE('',*,*,#4968,.T.);
#6678=ORIENTED_EDGE('',*,*,#4970,.T.);
#6679=ORIENTED_EDGE('',*,*,#4971,.T.);
#6680=ORIENTED_EDGE('',*,*,#4972,.T.);
#6681=ORIENTED_EDGE('',*,*,#4973,.F.);
#6682=ORIENTED_EDGE('',*,*,#4974,.T.);
#6683=ORIENTED_EDGE('',*,*,#4975,.T.);
#6684=ORIENTED_EDGE('',*,*,#4976,.T.);
#6685=ORIENTED_EDGE('',*,*,#4971,.F.);
#6686=ORIENTED_EDGE('',*,*,#4977,.T.);
#6687=ORIENTED_EDGE('',*,*,#4978,.T.);
#6688=ORIENTED_EDGE('',*,*,#4979,.T.);
#6689=ORIENTED_EDGE('',*,*,#4975,.F.);
#6690=ORIENTED_EDGE('',*,*,#4980,.T.);
#6691=ORIENTED_EDGE('',*,*,#4981,.T.);
#6692=ORIENTED_EDGE('',*,*,#4982,.T.);
#6693=ORIENTED_EDGE('',*,*,#4978,.F.);
#6694=ORIENTED_EDGE('',*,*,#4983,.T.);
#6695=ORIENTED_EDGE('',*,*,#4984,.T.);
#6696=ORIENTED_EDGE('',*,*,#4985,.T.);
#6697=ORIENTED_EDGE('',*,*,#4981,.F.);
#6698=ORIENTED_EDGE('',*,*,#4986,.T.);
#6699=ORIENTED_EDGE('',*,*,#4973,.T.);
#6700=ORIENTED_EDGE('',*,*,#4987,.T.);
#6701=ORIENTED_EDGE('',*,*,#4984,.F.);
#6702=ORIENTED_EDGE('',*,*,#4986,.F.);
#6703=ORIENTED_EDGE('',*,*,#4983,.F.);
#6704=ORIENTED_EDGE('',*,*,#4980,.F.);
#6705=ORIENTED_EDGE('',*,*,#4977,.F.);
#6706=ORIENTED_EDGE('',*,*,#4974,.F.);
#6707=ORIENTED_EDGE('',*,*,#4970,.F.);
#6708=ORIENTED_EDGE('',*,*,#4987,.F.);
#6709=ORIENTED_EDGE('',*,*,#4972,.F.);
#6710=ORIENTED_EDGE('',*,*,#4976,.F.);
#6711=ORIENTED_EDGE('',*,*,#4979,.F.);
#6712=ORIENTED_EDGE('',*,*,#4982,.F.);
#6713=ORIENTED_EDGE('',*,*,#4985,.F.);
#6714=CYLINDRICAL_SURFACE('',#7941,0.21);
#6715=CYLINDRICAL_SURFACE('',#7944,0.21);
#6716=CYLINDRICAL_SURFACE('',#7947,0.21);
#6717=CYLINDRICAL_SURFACE('',#7950,0.21);
#6718=CYLINDRICAL_SURFACE('',#7974,0.164999999999999);
#6719=CYLINDRICAL_SURFACE('',#7978,0.165);
#6720=CYLINDRICAL_SURFACE('',#7981,0.165);
#6721=CYLINDRICAL_SURFACE('',#7984,0.165);
#6722=CYLINDRICAL_SURFACE('',#7987,0.505);
#6723=CYLINDRICAL_SURFACE('',#7990,0.165);
#6724=CYLINDRICAL_SURFACE('',#7993,0.165);
#6725=CYLINDRICAL_SURFACE('',#7996,0.165);
#6726=CYLINDRICAL_SURFACE('',#7999,0.505);
#6727=CYLINDRICAL_SURFACE('',#8002,0.275);
#6728=CYLINDRICAL_SURFACE('',#8005,0.275);
#6729=CYLINDRICAL_SURFACE('',#8008,0.275);
#6730=CYLINDRICAL_SURFACE('',#8011,0.275);
#6731=CYLINDRICAL_SURFACE('',#8025,0.165);
#6732=CYLINDRICAL_SURFACE('',#8029,0.225);
#6733=CYLINDRICAL_SURFACE('',#8032,0.225);
#6734=CYLINDRICAL_SURFACE('',#8035,0.225);
#6735=CYLINDRICAL_SURFACE('',#8044,1.5);
#6736=CYLINDRICAL_SURFACE('',#8045,0.5);
#6737=CYLINDRICAL_SURFACE('',#8047,0.5);
#6738=CYLINDRICAL_SURFACE('',#8052,0.505);
#6739=CYLINDRICAL_SURFACE('',#8055,0.7);
#6740=CYLINDRICAL_SURFACE('',#8061,0.505);
#6741=CYLINDRICAL_SURFACE('',#8064,0.7);
#6742=CYLINDRICAL_SURFACE('',#8070,0.505);
#6743=CYLINDRICAL_SURFACE('',#8073,0.7);
#6744=CYLINDRICAL_SURFACE('',#8079,0.225);
#6745=CYLINDRICAL_SURFACE('',#8082,0.9);
#6746=CYLINDRICAL_SURFACE('',#8088,0.165);
#6747=CYLINDRICAL_SURFACE('',#8092,0.225);
#6748=CYLINDRICAL_SURFACE('',#8095,0.225);
#6749=CYLINDRICAL_SURFACE('',#8098,0.225);
#6750=CYLINDRICAL_SURFACE('',#8107,1.5);
#6751=CYLINDRICAL_SURFACE('',#8108,0.5);
#6752=CYLINDRICAL_SURFACE('',#8110,0.5);
#6753=CYLINDRICAL_SURFACE('',#8115,0.505);
#6754=CYLINDRICAL_SURFACE('',#8118,0.7);
#6755=CYLINDRICAL_SURFACE('',#8124,0.505);
#6756=CYLINDRICAL_SURFACE('',#8127,0.7);
#6757=CYLINDRICAL_SURFACE('',#8133,0.505);
#6758=CYLINDRICAL_SURFACE('',#8136,0.7);
#6759=CYLINDRICAL_SURFACE('',#8142,0.225);
#6760=CYLINDRICAL_SURFACE('',#8145,0.9);
#6761=CYLINDRICAL_SURFACE('',#8151,0.225);
#6762=CYLINDRICAL_SURFACE('',#8154,0.07);
#6763=CYLINDRICAL_SURFACE('',#8169,0.0599999999999996);
#6764=CYLINDRICAL_SURFACE('',#8177,0.0600000000000001);
#6765=CYLINDRICAL_SURFACE('',#8199,0.425);
#6766=CYLINDRICAL_SURFACE('',#8207,0.24505);
#6767=CYLINDRICAL_SURFACE('',#8210,0.164999999999999);
#6768=CYLINDRICAL_SURFACE('',#8213,0.164999999999999);
#6769=CYLINDRICAL_SURFACE('',#8216,0.164999999999999);
#6770=CYLINDRICAL_SURFACE('',#8219,0.164999999999999);
#6771=CYLINDRICAL_SURFACE('',#8222,0.165);
#6772=CYLINDRICAL_SURFACE('',#8225,0.165);
#6773=CYLINDRICAL_SURFACE('',#8228,0.165);
#6774=CYLINDRICAL_SURFACE('',#8231,0.165);
#6775=CYLINDRICAL_SURFACE('',#8234,1.5);
#6776=CYLINDRICAL_SURFACE('',#8237,1.5);
#6777=CYLINDRICAL_SURFACE('',#8240,2.2);
#6778=CYLINDRICAL_SURFACE('',#8247,2.2);
#6779=CYLINDRICAL_SURFACE('',#8251,1.02);
#6780=CYLINDRICAL_SURFACE('',#8254,1.49);
#6781=CYLINDRICAL_SURFACE('',#8260,0.225);
#6782=CYLINDRICAL_SURFACE('',#8263,0.225);
#6783=CYLINDRICAL_SURFACE('',#8266,0.225);
#6784=CYLINDRICAL_SURFACE('',#8269,0.225);
#6785=CYLINDRICAL_SURFACE('',#8272,1.02);
#6786=CYLINDRICAL_SURFACE('',#8275,2.2);
#6787=CYLINDRICAL_SURFACE('',#8281,0.225);
#6788=CYLINDRICAL_SURFACE('',#8284,0.225);
#6789=CYLINDRICAL_SURFACE('',#8287,0.225);
#6790=CYLINDRICAL_SURFACE('',#8290,0.225);
#6791=CYLINDRICAL_SURFACE('',#8293,1.02);
#6792=CYLINDRICAL_SURFACE('',#8296,2.2);
#6793=CYLINDRICAL_SURFACE('',#8302,1.02);
#6794=CYLINDRICAL_SURFACE('',#8305,1.49);
#6795=CYLINDRICAL_SURFACE('',#8311,0.225000000000001);
#6796=CYLINDRICAL_SURFACE('',#8314,0.225000000000001);
#6797=CYLINDRICAL_SURFACE('',#8317,0.225000000000001);
#6798=CYLINDRICAL_SURFACE('',#8320,0.225000000000001);
#6799=CYLINDRICAL_SURFACE('',#8323,1.02);
#6800=CYLINDRICAL_SURFACE('',#8326,2.2);
#6801=CYLINDRICAL_SURFACE('',#8332,0.225000000000001);
#6802=CYLINDRICAL_SURFACE('',#8335,0.225000000000001);
#6803=CYLINDRICAL_SURFACE('',#8338,0.225000000000001);
#6804=CYLINDRICAL_SURFACE('',#8341,0.225000000000001);
#6805=CYLINDRICAL_SURFACE('',#8344,1.02);
#6806=CYLINDRICAL_SURFACE('',#8347,2.2);
#6807=CYLINDRICAL_SURFACE('',#8353,0.0700000000000003);
#6808=CYLINDRICAL_SURFACE('',#8364,0.164999999999999);
#6809=CYLINDRICAL_SURFACE('',#8367,0.164999999999999);
#6810=CYLINDRICAL_SURFACE('',#8370,0.164999999999999);
#6811=CYLINDRICAL_SURFACE('',#8373,0.164999999999999);
#6812=CYLINDRICAL_SURFACE('',#8376,0.165);
#6813=CYLINDRICAL_SURFACE('',#8379,0.165);
#6814=CYLINDRICAL_SURFACE('',#8382,0.165);
#6815=CYLINDRICAL_SURFACE('',#8385,0.165);
#6816=CYLINDRICAL_SURFACE('',#8388,1.5);
#6817=CYLINDRICAL_SURFACE('',#8391,1.5);
#6818=CYLINDRICAL_SURFACE('',#8394,2.2);
#6819=CYLINDRICAL_SURFACE('',#8401,2.2);
#6820=CYLINDRICAL_SURFACE('',#8405,1.02);
#6821=CYLINDRICAL_SURFACE('',#8408,1.49);
#6822=CYLINDRICAL_SURFACE('',#8414,0.225);
#6823=CYLINDRICAL_SURFACE('',#8417,0.225);
#6824=CYLINDRICAL_SURFACE('',#8420,0.225);
#6825=CYLINDRICAL_SURFACE('',#8423,0.225);
#6826=CYLINDRICAL_SURFACE('',#8426,1.02);
#6827=CYLINDRICAL_SURFACE('',#8429,2.2);
#6828=CYLINDRICAL_SURFACE('',#8435,0.225);
#6829=CYLINDRICAL_SURFACE('',#8438,0.225);
#6830=CYLINDRICAL_SURFACE('',#8441,0.225);
#6831=CYLINDRICAL_SURFACE('',#8444,0.225);
#6832=CYLINDRICAL_SURFACE('',#8447,1.02);
#6833=CYLINDRICAL_SURFACE('',#8450,2.2);
#6834=CYLINDRICAL_SURFACE('',#8456,1.02);
#6835=CYLINDRICAL_SURFACE('',#8459,1.49);
#6836=CYLINDRICAL_SURFACE('',#8465,0.225000000000001);
#6837=CYLINDRICAL_SURFACE('',#8468,0.225000000000001);
#6838=CYLINDRICAL_SURFACE('',#8471,0.225000000000001);
#6839=CYLINDRICAL_SURFACE('',#8474,0.225000000000001);
#6840=CYLINDRICAL_SURFACE('',#8477,1.02);
#6841=CYLINDRICAL_SURFACE('',#8480,2.2);
#6842=CYLINDRICAL_SURFACE('',#8486,0.225000000000001);
#6843=CYLINDRICAL_SURFACE('',#8489,0.225000000000001);
#6844=CYLINDRICAL_SURFACE('',#8492,0.225000000000001);
#6845=CYLINDRICAL_SURFACE('',#8495,0.225000000000001);
#6846=CYLINDRICAL_SURFACE('',#8498,1.02);
#6847=CYLINDRICAL_SURFACE('',#8501,2.2);
#6848=CYLINDRICAL_SURFACE('',#8514,0.976185);
#6849=CYLINDRICAL_SURFACE('',#8516,0.5);
#6850=CYLINDRICAL_SURFACE('',#8522,0.976185);
#6851=CYLINDRICAL_SURFACE('',#8534,1.023815);
#6852=CYLINDRICAL_SURFACE('',#8541,1.5);
#6853=CYLINDRICAL_SURFACE('',#8546,1.023815);
#6854=CYLINDRICAL_SURFACE('',#8568,1.019052);
#6855=CYLINDRICAL_SURFACE('',#8608,0.980948);
#6856=CYLINDRICAL_SURFACE('',#8622,1.013815);
#6857=CYLINDRICAL_SURFACE('',#8626,0.991185);
#6858=CYLINDRICAL_SURFACE('',#8630,1.013815);
#6859=CYLINDRICAL_SURFACE('',#8634,0.991185);
#6860=CYLINDRICAL_SURFACE('',#8655,0.35);
#6861=CYLINDRICAL_SURFACE('',#8663,0.1954);
#6862=CYLINDRICAL_SURFACE('',#8721,0.164999999999999);
#6863=CYLINDRICAL_SURFACE('',#8724,0.164999999999999);
#6864=CYLINDRICAL_SURFACE('',#8727,0.164999999999999);
#6865=CYLINDRICAL_SURFACE('',#8730,0.504999999999999);
#6866=CYLINDRICAL_SURFACE('',#8733,0.164999999999999);
#6867=CYLINDRICAL_SURFACE('',#8736,0.164999999999999);
#6868=CYLINDRICAL_SURFACE('',#8739,0.164999999999999);
#6869=CYLINDRICAL_SURFACE('',#8742,0.504999999999999);
#6870=CYLINDRICAL_SURFACE('',#8745,0.329999999999998);
#6871=CYLINDRICAL_SURFACE('',#8748,0.329999999999998);
#6872=CYLINDRICAL_SURFACE('',#8751,0.329999999999998);
#6873=CYLINDRICAL_SURFACE('',#8754,0.329999999999998);
#6874=CYLINDRICAL_SURFACE('',#8767,0.164999999999999);
#6875=CYLINDRICAL_SURFACE('',#8771,0.225000000000001);
#6876=CYLINDRICAL_SURFACE('',#8774,0.225000000000001);
#6877=CYLINDRICAL_SURFACE('',#8777,0.225000000000001);
#6878=CYLINDRICAL_SURFACE('',#8786,1.5);
#6879=CYLINDRICAL_SURFACE('',#8787,0.5);
#6880=CYLINDRICAL_SURFACE('',#8789,0.5);
#6881=CYLINDRICAL_SURFACE('',#8794,0.504999999999999);
#6882=CYLINDRICAL_SURFACE('',#8797,0.699999999999999);
#6883=CYLINDRICAL_SURFACE('',#8803,0.504999999999999);
#6884=CYLINDRICAL_SURFACE('',#8806,0.699999999999999);
#6885=CYLINDRICAL_SURFACE('',#8812,0.504999999999999);
#6886=CYLINDRICAL_SURFACE('',#8815,0.699999999999999);
#6887=CYLINDRICAL_SURFACE('',#8821,0.225000000000001);
#6888=CYLINDRICAL_SURFACE('',#8824,0.899999999999999);
#6889=CYLINDRICAL_SURFACE('',#8830,0.164999999999999);
#6890=CYLINDRICAL_SURFACE('',#8834,0.225000000000001);
#6891=CYLINDRICAL_SURFACE('',#8837,0.225000000000001);
#6892=CYLINDRICAL_SURFACE('',#8840,0.225000000000001);
#6893=CYLINDRICAL_SURFACE('',#8849,1.5);
#6894=CYLINDRICAL_SURFACE('',#8850,0.5);
#6895=CYLINDRICAL_SURFACE('',#8852,0.5);
#6896=CYLINDRICAL_SURFACE('',#8857,0.504999999999999);
#6897=CYLINDRICAL_SURFACE('',#8860,0.699999999999999);
#6898=CYLINDRICAL_SURFACE('',#8866,0.504999999999999);
#6899=CYLINDRICAL_SURFACE('',#8869,0.699999999999999);
#6900=CYLINDRICAL_SURFACE('',#8875,0.504999999999999);
#6901=CYLINDRICAL_SURFACE('',#8878,0.699999999999999);
#6902=CYLINDRICAL_SURFACE('',#8884,0.225000000000001);
#6903=CYLINDRICAL_SURFACE('',#8887,0.899999999999999);
#6904=CYLINDRICAL_SURFACE('',#8897,0.35);
#6905=CYLINDRICAL_SURFACE('',#8905,0.1954);
#6906=ADVANCED_FACE('',(#1201),#6714,.F.);
#6907=ADVANCED_FACE('',(#1202),#6715,.F.);
#6908=ADVANCED_FACE('',(#1203),#6716,.F.);
#6909=ADVANCED_FACE('',(#1204),#6717,.F.);
#6910=ADVANCED_FACE('',(#1205),#1006,.T.);
#6911=ADVANCED_FACE('',(#1206),#1007,.T.);
#6912=ADVANCED_FACE('',(#1207),#1008,.T.);
#6913=ADVANCED_FACE('',(#1208),#1009,.T.);
#6914=ADVANCED_FACE('',(#1209,#735,#736,#737,#738),#1010,.T.);
#6915=ADVANCED_FACE('',(#1210,#739,#740,#741,#742),#1011,.F.);
#6916=ADVANCED_FACE('',(#1211),#1012,.T.);
#6917=ADVANCED_FACE('',(#1212),#1013,.T.);
#6918=ADVANCED_FACE('',(#1213),#1014,.T.);
#6919=ADVANCED_FACE('',(#1214),#1015,.T.);
#6920=ADVANCED_FACE('',(#1215),#1016,.T.);
#6921=ADVANCED_FACE('',(#1216),#1017,.F.);
#6922=ADVANCED_FACE('',(#1217),#1018,.T.);
#6923=ADVANCED_FACE('',(#1218),#1019,.T.);
#6924=ADVANCED_FACE('',(#1219),#1020,.T.);
#6925=ADVANCED_FACE('',(#1220),#1021,.T.);
#6926=ADVANCED_FACE('',(#1221),#1022,.T.);
#6927=ADVANCED_FACE('',(#1222),#1023,.F.);
#6928=ADVANCED_FACE('',(#1223),#6718,.F.);
#6929=ADVANCED_FACE('',(#1224),#1024,.F.);
#6930=ADVANCED_FACE('',(#1225),#6719,.F.);
#6931=ADVANCED_FACE('',(#1226),#6720,.F.);
#6932=ADVANCED_FACE('',(#1227),#6721,.F.);
#6933=ADVANCED_FACE('',(#1228),#6722,.F.);
#6934=ADVANCED_FACE('',(#1229),#6723,.F.);
#6935=ADVANCED_FACE('',(#1230),#6724,.F.);
#6936=ADVANCED_FACE('',(#1231),#6725,.F.);
#6937=ADVANCED_FACE('',(#1232),#6726,.F.);
#6938=ADVANCED_FACE('',(#1233),#6727,.F.);
#6939=ADVANCED_FACE('',(#1234),#6728,.F.);
#6940=ADVANCED_FACE('',(#1235),#6729,.F.);
#6941=ADVANCED_FACE('',(#1236),#6730,.F.);
#6942=ADVANCED_FACE('',(#1237,#743,#744,#745,#746),#1025,.T.);
#6943=ADVANCED_FACE('',(#1238),#1026,.T.);
#6944=ADVANCED_FACE('',(#1239,#747,#748,#749,#750),#1027,.T.);
#6945=ADVANCED_FACE('',(#1240),#1028,.T.);
#6946=ADVANCED_FACE('',(#1241),#1029,.T.);
#6947=ADVANCED_FACE('',(#1242,#751,#752,#753,#754,#755,#756,#757,#758),
#1030,.T.);
#6948=ADVANCED_FACE('',(#1243),#1031,.T.);
#6949=ADVANCED_FACE('',(#1244,#759,#760,#761,#762,#763,#764,#765,#766),
#1032,.T.);
#6950=ADVANCED_FACE('',(#1245,#767),#1033,.T.);
#6951=ADVANCED_FACE('',(#1246),#1034,.T.);
#6952=ADVANCED_FACE('',(#1247),#6731,.F.);
#6953=ADVANCED_FACE('',(#1248),#1035,.F.);
#6954=ADVANCED_FACE('',(#1249),#6732,.F.);
#6955=ADVANCED_FACE('',(#1250),#6733,.F.);
#6956=ADVANCED_FACE('',(#1251),#6734,.F.);
#6957=ADVANCED_FACE('',(#1252,#768,#769,#770,#771),#1036,.T.);
#6958=ADVANCED_FACE('',(#1253,#772,#773,#774,#775),#1037,.F.);
#6959=ADVANCED_FACE('',(#1254),#6735,.T.);
#6960=ADVANCED_FACE('',(#1255),#6736,.T.);
#6961=ADVANCED_FACE('',(#1256),#6737,.T.);
#6962=ADVANCED_FACE('',(#1257),#1038,.T.);
#6963=ADVANCED_FACE('',(#1258,#776),#1039,.F.);
#6964=ADVANCED_FACE('',(#1259),#6738,.F.);
#6965=ADVANCED_FACE('',(#1260),#6739,.T.);
#6966=ADVANCED_FACE('',(#1261,#777),#1040,.T.);
#6967=ADVANCED_FACE('',(#1262,#778),#1041,.F.);
#6968=ADVANCED_FACE('',(#1263),#6740,.F.);
#6969=ADVANCED_FACE('',(#1264),#6741,.T.);
#6970=ADVANCED_FACE('',(#1265,#779),#1042,.T.);
#6971=ADVANCED_FACE('',(#1266,#780),#1043,.F.);
#6972=ADVANCED_FACE('',(#1267),#6742,.F.);
#6973=ADVANCED_FACE('',(#1268),#6743,.T.);
#6974=ADVANCED_FACE('',(#1269,#781),#1044,.T.);
#6975=ADVANCED_FACE('',(#1270,#782),#1045,.F.);
#6976=ADVANCED_FACE('',(#1271),#6744,.F.);
#6977=ADVANCED_FACE('',(#1272),#6745,.T.);
#6978=ADVANCED_FACE('',(#1273,#783),#1046,.T.);
#6979=ADVANCED_FACE('',(#1274,#784),#1047,.F.);
#6980=ADVANCED_FACE('',(#1275),#6746,.F.);
#6981=ADVANCED_FACE('',(#1276),#1048,.F.);
#6982=ADVANCED_FACE('',(#1277),#6747,.F.);
#6983=ADVANCED_FACE('',(#1278),#6748,.F.);
#6984=ADVANCED_FACE('',(#1279),#6749,.F.);
#6985=ADVANCED_FACE('',(#1280,#785,#786,#787,#788),#1049,.T.);
#6986=ADVANCED_FACE('',(#1281,#789,#790,#791,#792),#1050,.F.);
#6987=ADVANCED_FACE('',(#1282),#6750,.T.);
#6988=ADVANCED_FACE('',(#1283),#6751,.T.);
#6989=ADVANCED_FACE('',(#1284),#6752,.T.);
#6990=ADVANCED_FACE('',(#1285),#1051,.T.);
#6991=ADVANCED_FACE('',(#1286,#793),#1052,.F.);
#6992=ADVANCED_FACE('',(#1287),#6753,.F.);
#6993=ADVANCED_FACE('',(#1288),#6754,.T.);
#6994=ADVANCED_FACE('',(#1289,#794),#1053,.T.);
#6995=ADVANCED_FACE('',(#1290,#795),#1054,.F.);
#6996=ADVANCED_FACE('',(#1291),#6755,.F.);
#6997=ADVANCED_FACE('',(#1292),#6756,.T.);
#6998=ADVANCED_FACE('',(#1293,#796),#1055,.T.);
#6999=ADVANCED_FACE('',(#1294,#797),#1056,.F.);
#7000=ADVANCED_FACE('',(#1295),#6757,.F.);
#7001=ADVANCED_FACE('',(#1296),#6758,.T.);
#7002=ADVANCED_FACE('',(#1297,#798),#1057,.T.);
#7003=ADVANCED_FACE('',(#1298,#799),#1058,.F.);
#7004=ADVANCED_FACE('',(#1299),#6759,.F.);
#7005=ADVANCED_FACE('',(#1300),#6760,.T.);
#7006=ADVANCED_FACE('',(#1301,#800),#1059,.T.);
#7007=ADVANCED_FACE('',(#1302,#801),#1060,.F.);
#7008=ADVANCED_FACE('',(#1303),#6761,.F.);
#7009=ADVANCED_FACE('',(#1304),#6762,.F.);
#7010=ADVANCED_FACE('',(#1305),#1061,.T.);
#7011=ADVANCED_FACE('',(#1306,#802),#1062,.T.);
#7012=ADVANCED_FACE('',(#1307),#1063,.T.);
#7013=ADVANCED_FACE('',(#1308),#1064,.T.);
#7014=ADVANCED_FACE('',(#1309),#1065,.T.);
#7015=ADVANCED_FACE('',(#1310),#1066,.T.);
#7016=ADVANCED_FACE('',(#1311,#803),#1067,.T.);
#7017=ADVANCED_FACE('',(#1312),#1068,.T.);
#7018=ADVANCED_FACE('',(#1313,#804),#1069,.T.);
#7019=ADVANCED_FACE('',(#1314),#1070,.T.);
#7020=ADVANCED_FACE('',(#1315,#805),#1071,.F.);
#7021=ADVANCED_FACE('',(#1316),#6763,.T.);
#7022=ADVANCED_FACE('',(#1317),#1072,.T.);
#7023=ADVANCED_FACE('',(#1318),#1073,.F.);
#7024=ADVANCED_FACE('',(#1319),#1074,.T.);
#7025=ADVANCED_FACE('',(#1320),#6764,.T.);
#7026=ADVANCED_FACE('',(#1321),#1075,.T.);
#7027=ADVANCED_FACE('',(#1322),#1076,.F.);
#7028=ADVANCED_FACE('',(#1323),#1077,.F.);
#7029=ADVANCED_FACE('',(#1324),#497,.T.);
#7030=ADVANCED_FACE('',(#1325),#1078,.F.);
#7031=ADVANCED_FACE('',(#1326),#1079,.F.);
#7032=ADVANCED_FACE('',(#1327),#1080,.F.);
#7033=ADVANCED_FACE('',(#1328),#1081,.F.);
#7034=ADVANCED_FACE('',(#1329),#1082,.F.);
#7035=ADVANCED_FACE('',(#1330),#1083,.F.);
#7036=ADVANCED_FACE('',(#1331),#1084,.F.);
#7037=ADVANCED_FACE('',(#1332),#1085,.F.);
#7038=ADVANCED_FACE('',(#1333),#1086,.F.);
#7039=ADVANCED_FACE('',(#1334),#1087,.T.);
#7040=ADVANCED_FACE('',(#1335),#477,.T.);
#7041=ADVANCED_FACE('',(#1336),#6765,.T.);
#7042=ADVANCED_FACE('',(#1337),#478,.T.);
#7043=ADVANCED_FACE('',(#1338,#806),#1088,.T.);
#7044=ADVANCED_FACE('',(#1339),#479,.T.);
#7045=ADVANCED_FACE('',(#1340),#6766,.T.);
#7046=ADVANCED_FACE('',(#1341),#6767,.F.);
#7047=ADVANCED_FACE('',(#1342),#6768,.F.);
#7048=ADVANCED_FACE('',(#1343),#6769,.F.);
#7049=ADVANCED_FACE('',(#1344),#6770,.F.);
#7050=ADVANCED_FACE('',(#1345),#6771,.F.);
#7051=ADVANCED_FACE('',(#1346),#6772,.F.);
#7052=ADVANCED_FACE('',(#1347),#6773,.F.);
#7053=ADVANCED_FACE('',(#1348),#6774,.F.);
#7054=ADVANCED_FACE('',(#1349),#6775,.F.);
#7055=ADVANCED_FACE('',(#1350),#6776,.F.);
#7056=ADVANCED_FACE('',(#1351),#6777,.T.);
#7057=ADVANCED_FACE('',(#1352),#1089,.T.);
#7058=ADVANCED_FACE('',(#1353,#807,#808,#809,#810,#811,#812,#813,#814,#815,
#816),#1090,.F.);
#7059=ADVANCED_FACE('',(#1354),#1091,.T.);
#7060=ADVANCED_FACE('',(#1355),#6778,.T.);
#7061=ADVANCED_FACE('',(#1356,#817,#818,#819,#820,#821,#822,#823,#824,#825,
#826),#1092,.T.);
#7062=ADVANCED_FACE('',(#1357),#6779,.F.);
#7063=ADVANCED_FACE('',(#1358),#6780,.T.);
#7064=ADVANCED_FACE('',(#1359,#827),#1093,.T.);
#7065=ADVANCED_FACE('',(#1360,#828),#1094,.F.);
#7066=ADVANCED_FACE('',(#1361),#6781,.F.);
#7067=ADVANCED_FACE('',(#1362),#6782,.F.);
#7068=ADVANCED_FACE('',(#1363),#6783,.F.);
#7069=ADVANCED_FACE('',(#1364),#6784,.F.);
#7070=ADVANCED_FACE('',(#1365),#6785,.F.);
#7071=ADVANCED_FACE('',(#1366),#6786,.T.);
#7072=ADVANCED_FACE('',(#1367,#829,#830,#831,#832,#833),#1095,.T.);
#7073=ADVANCED_FACE('',(#1368,#834,#835,#836,#837,#838),#1096,.F.);
#7074=ADVANCED_FACE('',(#1369),#6787,.F.);
#7075=ADVANCED_FACE('',(#1370),#6788,.F.);
#7076=ADVANCED_FACE('',(#1371),#6789,.F.);
#7077=ADVANCED_FACE('',(#1372),#6790,.F.);
#7078=ADVANCED_FACE('',(#1373),#6791,.F.);
#7079=ADVANCED_FACE('',(#1374),#6792,.T.);
#7080=ADVANCED_FACE('',(#1375,#839,#840,#841,#842,#843),#1097,.T.);
#7081=ADVANCED_FACE('',(#1376,#844,#845,#846,#847,#848),#1098,.F.);
#7082=ADVANCED_FACE('',(#1377),#6793,.F.);
#7083=ADVANCED_FACE('',(#1378),#6794,.T.);
#7084=ADVANCED_FACE('',(#1379,#849),#1099,.T.);
#7085=ADVANCED_FACE('',(#1380,#850),#1100,.F.);
#7086=ADVANCED_FACE('',(#1381),#6795,.F.);
#7087=ADVANCED_FACE('',(#1382),#6796,.F.);
#7088=ADVANCED_FACE('',(#1383),#6797,.F.);
#7089=ADVANCED_FACE('',(#1384),#6798,.F.);
#7090=ADVANCED_FACE('',(#1385),#6799,.F.);
#7091=ADVANCED_FACE('',(#1386),#6800,.T.);
#7092=ADVANCED_FACE('',(#1387,#851,#852,#853,#854,#855),#1101,.T.);
#7093=ADVANCED_FACE('',(#1388,#856,#857,#858,#859,#860),#1102,.F.);
#7094=ADVANCED_FACE('',(#1389),#6801,.F.);
#7095=ADVANCED_FACE('',(#1390),#6802,.F.);
#7096=ADVANCED_FACE('',(#1391),#6803,.F.);
#7097=ADVANCED_FACE('',(#1392),#6804,.F.);
#7098=ADVANCED_FACE('',(#1393),#6805,.F.);
#7099=ADVANCED_FACE('',(#1394),#6806,.T.);
#7100=ADVANCED_FACE('',(#1395,#861,#862,#863,#864,#865),#1103,.T.);
#7101=ADVANCED_FACE('',(#1396,#866,#867,#868,#869,#870),#1104,.F.);
#7102=ADVANCED_FACE('',(#1397),#6807,.F.);
#7103=ADVANCED_FACE('',(#1398),#1105,.T.);
#7104=ADVANCED_FACE('',(#1399,#871),#1106,.T.);
#7105=ADVANCED_FACE('',(#1400),#1107,.T.);
#7106=ADVANCED_FACE('',(#1401,#872),#1108,.T.);
#7107=ADVANCED_FACE('',(#1402),#1109,.T.);
#7108=ADVANCED_FACE('',(#1403),#1110,.F.);
#7109=ADVANCED_FACE('',(#1404),#6808,.F.);
#7110=ADVANCED_FACE('',(#1405),#6809,.F.);
#7111=ADVANCED_FACE('',(#1406),#6810,.F.);
#7112=ADVANCED_FACE('',(#1407),#6811,.F.);
#7113=ADVANCED_FACE('',(#1408),#6812,.F.);
#7114=ADVANCED_FACE('',(#1409),#6813,.F.);
#7115=ADVANCED_FACE('',(#1410),#6814,.F.);
#7116=ADVANCED_FACE('',(#1411),#6815,.F.);
#7117=ADVANCED_FACE('',(#1412),#6816,.F.);
#7118=ADVANCED_FACE('',(#1413),#6817,.F.);
#7119=ADVANCED_FACE('',(#1414),#6818,.T.);
#7120=ADVANCED_FACE('',(#1415),#1111,.T.);
#7121=ADVANCED_FACE('',(#1416,#873,#874,#875,#876,#877,#878,#879,#880,#881,
#882),#1112,.F.);
#7122=ADVANCED_FACE('',(#1417),#1113,.T.);
#7123=ADVANCED_FACE('',(#1418),#6819,.T.);
#7124=ADVANCED_FACE('',(#1419,#883,#884,#885,#886,#887,#888,#889,#890,#891,
#892),#1114,.T.);
#7125=ADVANCED_FACE('',(#1420),#6820,.F.);
#7126=ADVANCED_FACE('',(#1421),#6821,.T.);
#7127=ADVANCED_FACE('',(#1422,#893),#1115,.T.);
#7128=ADVANCED_FACE('',(#1423,#894),#1116,.F.);
#7129=ADVANCED_FACE('',(#1424),#6822,.F.);
#7130=ADVANCED_FACE('',(#1425),#6823,.F.);
#7131=ADVANCED_FACE('',(#1426),#6824,.F.);
#7132=ADVANCED_FACE('',(#1427),#6825,.F.);
#7133=ADVANCED_FACE('',(#1428),#6826,.F.);
#7134=ADVANCED_FACE('',(#1429),#6827,.T.);
#7135=ADVANCED_FACE('',(#1430,#895,#896,#897,#898,#899),#1117,.T.);
#7136=ADVANCED_FACE('',(#1431,#900,#901,#902,#903,#904),#1118,.F.);
#7137=ADVANCED_FACE('',(#1432),#6828,.F.);
#7138=ADVANCED_FACE('',(#1433),#6829,.F.);
#7139=ADVANCED_FACE('',(#1434),#6830,.F.);
#7140=ADVANCED_FACE('',(#1435),#6831,.F.);
#7141=ADVANCED_FACE('',(#1436),#6832,.F.);
#7142=ADVANCED_FACE('',(#1437),#6833,.T.);
#7143=ADVANCED_FACE('',(#1438,#905,#906,#907,#908,#909),#1119,.T.);
#7144=ADVANCED_FACE('',(#1439,#910,#911,#912,#913,#914),#1120,.F.);
#7145=ADVANCED_FACE('',(#1440),#6834,.F.);
#7146=ADVANCED_FACE('',(#1441),#6835,.T.);
#7147=ADVANCED_FACE('',(#1442,#915),#1121,.T.);
#7148=ADVANCED_FACE('',(#1443,#916),#1122,.F.);
#7149=ADVANCED_FACE('',(#1444),#6836,.F.);
#7150=ADVANCED_FACE('',(#1445),#6837,.F.);
#7151=ADVANCED_FACE('',(#1446),#6838,.F.);
#7152=ADVANCED_FACE('',(#1447),#6839,.F.);
#7153=ADVANCED_FACE('',(#1448),#6840,.F.);
#7154=ADVANCED_FACE('',(#1449),#6841,.T.);
#7155=ADVANCED_FACE('',(#1450,#917,#918,#919,#920,#921),#1123,.T.);
#7156=ADVANCED_FACE('',(#1451,#922,#923,#924,#925,#926),#1124,.F.);
#7157=ADVANCED_FACE('',(#1452),#6842,.F.);
#7158=ADVANCED_FACE('',(#1453),#6843,.F.);
#7159=ADVANCED_FACE('',(#1454),#6844,.F.);
#7160=ADVANCED_FACE('',(#1455),#6845,.F.);
#7161=ADVANCED_FACE('',(#1456),#6846,.F.);
#7162=ADVANCED_FACE('',(#1457),#6847,.T.);
#7163=ADVANCED_FACE('',(#1458,#927,#928,#929,#930,#931),#1125,.T.);
#7164=ADVANCED_FACE('',(#1459,#932,#933,#934,#935,#936),#1126,.F.);
#7165=ADVANCED_FACE('',(#1460),#475,.F.);
#7166=ADVANCED_FACE('',(#1461),#6848,.T.);
#7167=ADVANCED_FACE('',(#1462),#6849,.F.);
#7168=ADVANCED_FACE('',(#1463),#480,.F.);
#7169=ADVANCED_FACE('',(#1464,#937),#1127,.T.);
#7170=ADVANCED_FACE('',(#1465),#6850,.T.);
#7171=ADVANCED_FACE('',(#1466,#938),#1128,.T.);
#7172=ADVANCED_FACE('',(#1467),#481,.F.);
#7173=ADVANCED_FACE('',(#1468),#476,.F.);
#7174=ADVANCED_FACE('',(#1469),#6851,.F.);
#7175=ADVANCED_FACE('',(#1470,#939),#1129,.T.);
#7176=ADVANCED_FACE('',(#1471),#482,.T.);
#7177=ADVANCED_FACE('',(#1472),#6852,.T.);
#7178=ADVANCED_FACE('',(#1473),#483,.T.);
#7179=ADVANCED_FACE('',(#1474,#940),#1130,.T.);
#7180=ADVANCED_FACE('',(#1475),#6853,.F.);
#7181=ADVANCED_FACE('',(#1476),#459,.T.);
#7182=ADVANCED_FACE('',(#1477),#460,.T.);
#7183=ADVANCED_FACE('',(#1478),#461,.T.);
#7184=ADVANCED_FACE('',(#1479),#462,.T.);
#7185=ADVANCED_FACE('',(#1480),#463,.T.);
#7186=ADVANCED_FACE('',(#1481),#464,.T.);
#7187=ADVANCED_FACE('',(#1482),#465,.T.);
#7188=ADVANCED_FACE('',(#1483),#466,.T.);
#7189=ADVANCED_FACE('',(#1484),#467,.F.);
#7190=ADVANCED_FACE('',(#1485),#6854,.T.);
#7191=ADVANCED_FACE('',(#1486),#1131,.T.);
#7192=ADVANCED_FACE('',(#1487),#468,.F.);
#7193=ADVANCED_FACE('',(#1488),#1132,.T.);
#7194=ADVANCED_FACE('',(#1489),#469,.F.);
#7195=ADVANCED_FACE('',(#1490),#1133,.T.);
#7196=ADVANCED_FACE('',(#1491),#470,.F.);
#7197=ADVANCED_FACE('',(#1492),#1134,.T.);
#7198=ADVANCED_FACE('',(#1493),#471,.F.);
#7199=ADVANCED_FACE('',(#1494),#1135,.T.);
#7200=ADVANCED_FACE('',(#1495),#472,.F.);
#7201=ADVANCED_FACE('',(#1496),#1136,.T.);
#7202=ADVANCED_FACE('',(#1497),#473,.F.);
#7203=ADVANCED_FACE('',(#1498),#6855,.F.);
#7204=ADVANCED_FACE('',(#1499),#1137,.T.);
#7205=ADVANCED_FACE('',(#1500),#474,.F.);
#7206=ADVANCED_FACE('',(#1501,#941),#1138,.T.);
#7207=ADVANCED_FACE('',(#1502),#1139,.T.);
#7208=ADVANCED_FACE('',(#1503,#942),#1140,.T.);
#7209=ADVANCED_FACE('',(#1504),#6856,.T.);
#7210=ADVANCED_FACE('',(#1505,#943),#1141,.T.);
#7211=ADVANCED_FACE('',(#1506),#6857,.F.);
#7212=ADVANCED_FACE('',(#1507,#944),#1142,.T.);
#7213=ADVANCED_FACE('',(#1508),#6858,.T.);
#7214=ADVANCED_FACE('',(#1509,#945),#1143,.T.);
#7215=ADVANCED_FACE('',(#1510),#6859,.F.);
#7216=ADVANCED_FACE('',(#1511),#1144,.F.);
#7217=ADVANCED_FACE('',(#1512),#1145,.F.);
#7218=ADVANCED_FACE('',(#1513),#1146,.F.);
#7219=ADVANCED_FACE('',(#1514),#1147,.F.);
#7220=ADVANCED_FACE('',(#1515),#1148,.F.);
#7221=ADVANCED_FACE('',(#1516),#1149,.F.);
#7222=ADVANCED_FACE('',(#1517),#1150,.F.);
#7223=ADVANCED_FACE('',(#1518),#1151,.F.);
#7224=ADVANCED_FACE('',(#1519),#1152,.F.);
#7225=ADVANCED_FACE('',(#1520),#1153,.T.);
#7226=ADVANCED_FACE('',(#1521),#484,.T.);
#7227=ADVANCED_FACE('',(#1522),#6860,.T.);
#7228=ADVANCED_FACE('',(#1523),#485,.T.);
#7229=ADVANCED_FACE('',(#1524,#946),#1154,.T.);
#7230=ADVANCED_FACE('',(#1525),#486,.T.);
#7231=ADVANCED_FACE('',(#1526),#6861,.T.);
#7232=ADVANCED_FACE('',(#1527),#6862,.F.);
#7233=ADVANCED_FACE('',(#1528),#6863,.F.);
#7234=ADVANCED_FACE('',(#1529),#6864,.F.);
#7235=ADVANCED_FACE('',(#1530),#6865,.F.);
#7236=ADVANCED_FACE('',(#1531),#6866,.F.);
#7237=ADVANCED_FACE('',(#1532),#6867,.F.);
#7238=ADVANCED_FACE('',(#1533),#6868,.F.);
#7239=ADVANCED_FACE('',(#1534),#6869,.F.);
#7240=ADVANCED_FACE('',(#1535),#6870,.F.);
#7241=ADVANCED_FACE('',(#1536),#6871,.F.);
#7242=ADVANCED_FACE('',(#1537),#6872,.F.);
#7243=ADVANCED_FACE('',(#1538),#6873,.F.);
#7244=ADVANCED_FACE('',(#1539),#1155,.T.);
#7245=ADVANCED_FACE('',(#1540),#1156,.T.);
#7246=ADVANCED_FACE('',(#1541,#947,#948,#949,#950),#1157,.T.);
#7247=ADVANCED_FACE('',(#1542,#951,#952,#953,#954),#1158,.F.);
#7248=ADVANCED_FACE('',(#1543,#955,#956,#957,#958,#959,#960,#961,#962),
#1159,.T.);
#7249=ADVANCED_FACE('',(#1544),#1160,.T.);
#7250=ADVANCED_FACE('',(#1545,#963,#964,#965,#966,#967,#968,#969,#970),
#1161,.T.);
#7251=ADVANCED_FACE('',(#1546),#1162,.T.);
#7252=ADVANCED_FACE('',(#1547),#1163,.F.);
#7253=ADVANCED_FACE('',(#1548),#6874,.F.);
#7254=ADVANCED_FACE('',(#1549),#1164,.F.);
#7255=ADVANCED_FACE('',(#1550),#6875,.F.);
#7256=ADVANCED_FACE('',(#1551),#6876,.F.);
#7257=ADVANCED_FACE('',(#1552),#6877,.F.);
#7258=ADVANCED_FACE('',(#1553,#971,#972,#973,#974),#1165,.T.);
#7259=ADVANCED_FACE('',(#1554,#975,#976,#977,#978),#1166,.F.);
#7260=ADVANCED_FACE('',(#1555),#6878,.T.);
#7261=ADVANCED_FACE('',(#1556),#6879,.T.);
#7262=ADVANCED_FACE('',(#1557),#6880,.T.);
#7263=ADVANCED_FACE('',(#1558),#1167,.T.);
#7264=ADVANCED_FACE('',(#1559,#979),#1168,.F.);
#7265=ADVANCED_FACE('',(#1560),#6881,.F.);
#7266=ADVANCED_FACE('',(#1561),#6882,.T.);
#7267=ADVANCED_FACE('',(#1562,#980),#1169,.T.);
#7268=ADVANCED_FACE('',(#1563,#981),#1170,.F.);
#7269=ADVANCED_FACE('',(#1564),#6883,.F.);
#7270=ADVANCED_FACE('',(#1565),#6884,.T.);
#7271=ADVANCED_FACE('',(#1566,#982),#1171,.T.);
#7272=ADVANCED_FACE('',(#1567,#983),#1172,.F.);
#7273=ADVANCED_FACE('',(#1568),#6885,.F.);
#7274=ADVANCED_FACE('',(#1569),#6886,.T.);
#7275=ADVANCED_FACE('',(#1570,#984),#1173,.T.);
#7276=ADVANCED_FACE('',(#1571,#985),#1174,.F.);
#7277=ADVANCED_FACE('',(#1572),#6887,.F.);
#7278=ADVANCED_FACE('',(#1573),#6888,.T.);
#7279=ADVANCED_FACE('',(#1574,#986),#1175,.T.);
#7280=ADVANCED_FACE('',(#1575,#987),#1176,.F.);
#7281=ADVANCED_FACE('',(#1576),#6889,.F.);
#7282=ADVANCED_FACE('',(#1577),#1177,.F.);
#7283=ADVANCED_FACE('',(#1578),#6890,.F.);
#7284=ADVANCED_FACE('',(#1579),#6891,.F.);
#7285=ADVANCED_FACE('',(#1580),#6892,.F.);
#7286=ADVANCED_FACE('',(#1581,#988,#989,#990,#991),#1178,.T.);
#7287=ADVANCED_FACE('',(#1582,#992,#993,#994,#995),#1179,.F.);
#7288=ADVANCED_FACE('',(#1583),#6893,.T.);
#7289=ADVANCED_FACE('',(#1584),#6894,.T.);
#7290=ADVANCED_FACE('',(#1585),#6895,.T.);
#7291=ADVANCED_FACE('',(#1586),#1180,.T.);
#7292=ADVANCED_FACE('',(#1587,#996),#1181,.F.);
#7293=ADVANCED_FACE('',(#1588),#6896,.F.);
#7294=ADVANCED_FACE('',(#1589),#6897,.T.);
#7295=ADVANCED_FACE('',(#1590,#997),#1182,.T.);
#7296=ADVANCED_FACE('',(#1591,#998),#1183,.F.);
#7297=ADVANCED_FACE('',(#1592),#6898,.F.);
#7298=ADVANCED_FACE('',(#1593),#6899,.T.);
#7299=ADVANCED_FACE('',(#1594,#999),#1184,.T.);
#7300=ADVANCED_FACE('',(#1595,#1000),#1185,.F.);
#7301=ADVANCED_FACE('',(#1596),#6900,.F.);
#7302=ADVANCED_FACE('',(#1597),#6901,.T.);
#7303=ADVANCED_FACE('',(#1598,#1001),#1186,.T.);
#7304=ADVANCED_FACE('',(#1599,#1002),#1187,.F.);
#7305=ADVANCED_FACE('',(#1600),#6902,.F.);
#7306=ADVANCED_FACE('',(#1601),#6903,.T.);
#7307=ADVANCED_FACE('',(#1602,#1003),#1188,.T.);
#7308=ADVANCED_FACE('',(#1603,#1004),#1189,.F.);
#7309=ADVANCED_FACE('',(#1604),#1190,.T.);
#7310=ADVANCED_FACE('',(#1605),#487,.T.);
#7311=ADVANCED_FACE('',(#1606),#6904,.T.);
#7312=ADVANCED_FACE('',(#1607),#488,.T.);
#7313=ADVANCED_FACE('',(#1608,#1005),#1191,.T.);
#7314=ADVANCED_FACE('',(#1609),#489,.T.);
#7315=ADVANCED_FACE('',(#1610),#6905,.T.);
#7316=ADVANCED_FACE('',(#1611),#490,.T.);
#7317=ADVANCED_FACE('',(#1612),#1192,.T.);
#7318=ADVANCED_FACE('',(#1613),#1193,.F.);
#7319=ADVANCED_FACE('',(#1614),#1194,.F.);
#7320=ADVANCED_FACE('',(#1615),#1195,.F.);
#7321=ADVANCED_FACE('',(#1616),#1196,.F.);
#7322=ADVANCED_FACE('',(#1617),#1197,.F.);
#7323=ADVANCED_FACE('',(#1618),#1198,.F.);
#7324=ADVANCED_FACE('',(#1619),#1199,.F.);
#7325=ADVANCED_FACE('',(#1620),#1200,.F.);
#7326=CLOSED_SHELL('',(#6906,#6907,#6908,#6909,#6910,#6911,#6912,#6913,
#6914,#6915));
#7327=CLOSED_SHELL('',(#6916,#6917,#6918,#6919,#6920,#6921));
#7328=CLOSED_SHELL('',(#6922,#6923,#6924,#6925,#6926,#6927));
#7329=CLOSED_SHELL('',(#6928,#6929,#6930,#6931,#6932,#6933,#6934,#6935,
#6936,#6937,#6938,#6939,#6940,#6941,#6942,#6943,#6944,#6945,#6946,#6947,
#6948,#6949,#6950,#6951));
#7330=CLOSED_SHELL('',(#6952,#6953,#6954,#6955,#6956,#6957,#6958,#6959,
#6960,#6961,#6962,#6963));
#7331=CLOSED_SHELL('',(#6964,#6965,#6966,#6967));
#7332=CLOSED_SHELL('',(#6968,#6969,#6970,#6971));
#7333=CLOSED_SHELL('',(#6972,#6973,#6974,#6975));
#7334=CLOSED_SHELL('',(#6976,#6977,#6978,#6979));
#7335=CLOSED_SHELL('',(#6980,#6981,#6982,#6983,#6984,#6985,#6986,#6987,
#6988,#6989,#6990,#6991));
#7336=CLOSED_SHELL('',(#6992,#6993,#6994,#6995));
#7337=CLOSED_SHELL('',(#6996,#6997,#6998,#6999));
#7338=CLOSED_SHELL('',(#7000,#7001,#7002,#7003));
#7339=CLOSED_SHELL('',(#7004,#7005,#7006,#7007));
#7340=CLOSED_SHELL('',(#7008,#7009,#7010,#7011,#7012,#7013,#7014,#7015,
#7016,#7017,#7018,#7019,#7020));
#7341=CLOSED_SHELL('',(#7021,#7022,#7023,#7024,#7025,#7026,#7027,#7028,
#7029));
#7342=CLOSED_SHELL('',(#7030,#7031,#7032,#7033,#7034,#7035,#7036,#7037));
#7343=CLOSED_SHELL('',(#7038,#7039,#7040,#7041,#7042,#7043,#7044,#7045));
#7344=CLOSED_SHELL('',(#7046,#7047,#7048,#7049,#7050,#7051,#7052,#7053,
#7054,#7055,#7056,#7057,#7058,#7059,#7060,#7061));
#7345=CLOSED_SHELL('',(#7062,#7063,#7064,#7065));
#7346=CLOSED_SHELL('',(#7066,#7067,#7068,#7069,#7070,#7071,#7072,#7073));
#7347=CLOSED_SHELL('',(#7074,#7075,#7076,#7077,#7078,#7079,#7080,#7081));
#7348=CLOSED_SHELL('',(#7082,#7083,#7084,#7085));
#7349=CLOSED_SHELL('',(#7086,#7087,#7088,#7089,#7090,#7091,#7092,#7093));
#7350=CLOSED_SHELL('',(#7094,#7095,#7096,#7097,#7098,#7099,#7100,#7101));
#7351=CLOSED_SHELL('',(#7102,#7103,#7104,#7105,#7106,#7107,#7108));
#7352=CLOSED_SHELL('',(#7109,#7110,#7111,#7112,#7113,#7114,#7115,#7116,
#7117,#7118,#7119,#7120,#7121,#7122,#7123,#7124));
#7353=CLOSED_SHELL('',(#7125,#7126,#7127,#7128));
#7354=CLOSED_SHELL('',(#7129,#7130,#7131,#7132,#7133,#7134,#7135,#7136));
#7355=CLOSED_SHELL('',(#7137,#7138,#7139,#7140,#7141,#7142,#7143,#7144));
#7356=CLOSED_SHELL('',(#7145,#7146,#7147,#7148));
#7357=CLOSED_SHELL('',(#7149,#7150,#7151,#7152,#7153,#7154,#7155,#7156));
#7358=CLOSED_SHELL('',(#7157,#7158,#7159,#7160,#7161,#7162,#7163,#7164));
#7359=CLOSED_SHELL('',(#7165,#7166,#7167,#7168,#7169,#7170,#7171,#7172));
#7360=CLOSED_SHELL('',(#7173,#7174,#7175,#7176,#7177,#7178,#7179,#7180));
#7361=CLOSED_SHELL('',(#7181));
#7362=CLOSED_SHELL('',(#7182));
#7363=CLOSED_SHELL('',(#7183));
#7364=CLOSED_SHELL('',(#7184));
#7365=CLOSED_SHELL('',(#7185));
#7366=CLOSED_SHELL('',(#7186));
#7367=CLOSED_SHELL('',(#7187));
#7368=CLOSED_SHELL('',(#7188));
#7369=CLOSED_SHELL('',(#7189,#7190,#7191,#7192,#7193,#7194,#7195,#7196,
#7197,#7198,#7199,#7200,#7201,#7202,#7203,#7204,#7205,#7206,#7207));
#7370=CLOSED_SHELL('',(#7208,#7209,#7210,#7211));
#7371=CLOSED_SHELL('',(#7212,#7213,#7214,#7215));
#7372=CLOSED_SHELL('',(#7216,#7217,#7218,#7219,#7220,#7221,#7222,#7223));
#7373=CLOSED_SHELL('',(#7224,#7225,#7226,#7227,#7228,#7229,#7230,#7231));
#7374=CLOSED_SHELL('',(#7232,#7233,#7234,#7235,#7236,#7237,#7238,#7239,
#7240,#7241,#7242,#7243,#7244,#7245,#7246,#7247,#7248,#7249,#7250,#7251,
#7252));
#7375=CLOSED_SHELL('',(#7253,#7254,#7255,#7256,#7257,#7258,#7259,#7260,
#7261,#7262,#7263,#7264));
#7376=CLOSED_SHELL('',(#7265,#7266,#7267,#7268));
#7377=CLOSED_SHELL('',(#7269,#7270,#7271,#7272));
#7378=CLOSED_SHELL('',(#7273,#7274,#7275,#7276));
#7379=CLOSED_SHELL('',(#7277,#7278,#7279,#7280));
#7380=CLOSED_SHELL('',(#7281,#7282,#7283,#7284,#7285,#7286,#7287,#7288,
#7289,#7290,#7291,#7292));
#7381=CLOSED_SHELL('',(#7293,#7294,#7295,#7296));
#7382=CLOSED_SHELL('',(#7297,#7298,#7299,#7300));
#7383=CLOSED_SHELL('',(#7301,#7302,#7303,#7304));
#7384=CLOSED_SHELL('',(#7305,#7306,#7307,#7308));
#7385=CLOSED_SHELL('',(#7309,#7310,#7311,#7312,#7313,#7314,#7315,#7316,
#7317));
#7386=CLOSED_SHELL('',(#7318,#7319,#7320,#7321,#7322,#7323,#7324,#7325));
#7387=DERIVED_UNIT_ELEMENT(#7487,1.);
#7388=DERIVED_UNIT_ELEMENT(#14514,-3.);
#7389=DERIVED_UNIT_ELEMENT(#7487,1.);
#7390=DERIVED_UNIT_ELEMENT(#14514,-3.);
#7391=DERIVED_UNIT_ELEMENT(#7487,1.);
#7392=DERIVED_UNIT_ELEMENT(#14514,-3.);
#7393=DERIVED_UNIT_ELEMENT(#7487,1.);
#7394=DERIVED_UNIT_ELEMENT(#14514,-3.);
#7395=DERIVED_UNIT_ELEMENT(#7487,1.);
#7396=DERIVED_UNIT_ELEMENT(#14514,-3.);
#7397=DERIVED_UNIT_ELEMENT(#7487,1.);
#7398=DERIVED_UNIT_ELEMENT(#14514,-3.);
#7399=DERIVED_UNIT_ELEMENT(#7487,1.);
#7400=DERIVED_UNIT_ELEMENT(#14514,-3.);
#7401=DERIVED_UNIT_ELEMENT(#7487,1.);
#7402=DERIVED_UNIT_ELEMENT(#14514,-3.);
#7403=DERIVED_UNIT_ELEMENT(#7487,1.);
#7404=DERIVED_UNIT_ELEMENT(#14514,-3.);
#7405=DERIVED_UNIT_ELEMENT(#7487,1.);
#7406=DERIVED_UNIT_ELEMENT(#14514,-3.);
#7407=DERIVED_UNIT_ELEMENT(#7487,1.);
#7408=DERIVED_UNIT_ELEMENT(#14514,-3.);
#7409=DERIVED_UNIT_ELEMENT(#7487,1.);
#7410=DERIVED_UNIT_ELEMENT(#14514,-3.);
#7411=DERIVED_UNIT_ELEMENT(#7487,1.);
#7412=DERIVED_UNIT_ELEMENT(#14514,-3.);
#7413=DERIVED_UNIT_ELEMENT(#7487,1.);
#7414=DERIVED_UNIT_ELEMENT(#14514,-3.);
#7415=DERIVED_UNIT_ELEMENT(#7487,1.);
#7416=DERIVED_UNIT_ELEMENT(#14514,-3.);
#7417=DERIVED_UNIT_ELEMENT(#7487,1.);
#7418=DERIVED_UNIT_ELEMENT(#14514,-3.);
#7419=DERIVED_UNIT_ELEMENT(#7487,1.);
#7420=DERIVED_UNIT_ELEMENT(#14514,-3.);
#7421=DERIVED_UNIT_ELEMENT(#7487,1.);
#7422=DERIVED_UNIT_ELEMENT(#14514,-3.);
#7423=DERIVED_UNIT_ELEMENT(#7487,1.);
#7424=DERIVED_UNIT_ELEMENT(#14514,-3.);
#7425=DERIVED_UNIT_ELEMENT(#7487,1.);
#7426=DERIVED_UNIT_ELEMENT(#14514,-3.);
#7427=DERIVED_UNIT_ELEMENT(#7487,1.);
#7428=DERIVED_UNIT_ELEMENT(#14514,-3.);
#7429=DERIVED_UNIT_ELEMENT(#7487,1.);
#7430=DERIVED_UNIT_ELEMENT(#14514,-3.);
#7431=DERIVED_UNIT_ELEMENT(#7487,1.);
#7432=DERIVED_UNIT_ELEMENT(#14514,-3.);
#7433=DERIVED_UNIT_ELEMENT(#7487,1.);
#7434=DERIVED_UNIT_ELEMENT(#14514,-3.);
#7435=DERIVED_UNIT_ELEMENT(#7487,1.);
#7436=DERIVED_UNIT_ELEMENT(#14514,-3.);
#7437=DERIVED_UNIT_ELEMENT(#7487,1.);
#7438=DERIVED_UNIT_ELEMENT(#14514,-3.);
#7439=DERIVED_UNIT_ELEMENT(#7487,1.);
#7440=DERIVED_UNIT_ELEMENT(#14514,-3.);
#7441=DERIVED_UNIT_ELEMENT(#7487,1.);
#7442=DERIVED_UNIT_ELEMENT(#14514,-3.);
#7443=DERIVED_UNIT_ELEMENT(#7487,1.);
#7444=DERIVED_UNIT_ELEMENT(#14514,-3.);
#7445=DERIVED_UNIT_ELEMENT(#7487,1.);
#7446=DERIVED_UNIT_ELEMENT(#14514,-3.);
#7447=DERIVED_UNIT_ELEMENT(#7487,1.);
#7448=DERIVED_UNIT_ELEMENT(#14514,-3.);
#7449=DERIVED_UNIT_ELEMENT(#7487,1.);
#7450=DERIVED_UNIT_ELEMENT(#14514,-3.);
#7451=DERIVED_UNIT_ELEMENT(#7487,1.);
#7452=DERIVED_UNIT_ELEMENT(#14514,-3.);
#7453=DERIVED_UNIT_ELEMENT(#7487,1.);
#7454=DERIVED_UNIT_ELEMENT(#14514,-3.);
#7455=DERIVED_UNIT_ELEMENT(#7487,1.);
#7456=DERIVED_UNIT_ELEMENT(#14514,-3.);
#7457=DERIVED_UNIT_ELEMENT(#7487,1.);
#7458=DERIVED_UNIT_ELEMENT(#14514,-3.);
#7459=DERIVED_UNIT_ELEMENT(#7487,1.);
#7460=DERIVED_UNIT_ELEMENT(#14514,-3.);
#7461=DERIVED_UNIT_ELEMENT(#7487,1.);
#7462=DERIVED_UNIT_ELEMENT(#14514,-3.);
#7463=DERIVED_UNIT_ELEMENT(#7487,1.);
#7464=DERIVED_UNIT_ELEMENT(#14514,-3.);
#7465=DERIVED_UNIT_ELEMENT(#7487,1.);
#7466=DERIVED_UNIT_ELEMENT(#14514,-3.);
#7467=DERIVED_UNIT_ELEMENT(#7487,1.);
#7468=DERIVED_UNIT_ELEMENT(#14514,-3.);
#7469=DERIVED_UNIT_ELEMENT(#7487,1.);
#7470=DERIVED_UNIT_ELEMENT(#14514,-3.);
#7471=DERIVED_UNIT_ELEMENT(#7487,1.);
#7472=DERIVED_UNIT_ELEMENT(#14514,-3.);
#7473=DERIVED_UNIT_ELEMENT(#7487,1.);
#7474=DERIVED_UNIT_ELEMENT(#14514,-3.);
#7475=DERIVED_UNIT_ELEMENT(#7487,1.);
#7476=DERIVED_UNIT_ELEMENT(#14514,-3.);
#7477=DERIVED_UNIT_ELEMENT(#7487,1.);
#7478=DERIVED_UNIT_ELEMENT(#14514,-3.);
#7479=DERIVED_UNIT_ELEMENT(#7487,1.);
#7480=DERIVED_UNIT_ELEMENT(#14514,-3.);
#7481=DERIVED_UNIT_ELEMENT(#7487,1.);
#7482=DERIVED_UNIT_ELEMENT(#14514,-3.);
#7483=DERIVED_UNIT_ELEMENT(#7487,1.);
#7484=DERIVED_UNIT_ELEMENT(#14514,-3.);
#7485=DERIVED_UNIT_ELEMENT(#7487,1.);
#7486=DERIVED_UNIT_ELEMENT(#14514,-3.);
#7487=(
MASS_UNIT()
NAMED_UNIT(*)
SI_UNIT(.KILO.,.GRAM.)
);
#7488=DERIVED_UNIT((#7387,#7388));
#7489=DERIVED_UNIT((#7389,#7390));
#7490=DERIVED_UNIT((#7391,#7392));
#7491=DERIVED_UNIT((#7393,#7394));
#7492=DERIVED_UNIT((#7395,#7396));
#7493=DERIVED_UNIT((#7397,#7398));
#7494=DERIVED_UNIT((#7399,#7400));
#7495=DERIVED_UNIT((#7401,#7402));
#7496=DERIVED_UNIT((#7403,#7404));
#7497=DERIVED_UNIT((#7405,#7406));
#7498=DERIVED_UNIT((#7407,#7408));
#7499=DERIVED_UNIT((#7409,#7410));
#7500=DERIVED_UNIT((#7411,#7412));
#7501=DERIVED_UNIT((#7413,#7414));
#7502=DERIVED_UNIT((#7415,#7416));
#7503=DERIVED_UNIT((#7417,#7418));
#7504=DERIVED_UNIT((#7419,#7420));
#7505=DERIVED_UNIT((#7421,#7422));
#7506=DERIVED_UNIT((#7423,#7424));
#7507=DERIVED_UNIT((#7425,#7426));
#7508=DERIVED_UNIT((#7427,#7428));
#7509=DERIVED_UNIT((#7429,#7430));
#7510=DERIVED_UNIT((#7431,#7432));
#7511=DERIVED_UNIT((#7433,#7434));
#7512=DERIVED_UNIT((#7435,#7436));
#7513=DERIVED_UNIT((#7437,#7438));
#7514=DERIVED_UNIT((#7439,#7440));
#7515=DERIVED_UNIT((#7441,#7442));
#7516=DERIVED_UNIT((#7443,#7444));
#7517=DERIVED_UNIT((#7445,#7446));
#7518=DERIVED_UNIT((#7447,#7448));
#7519=DERIVED_UNIT((#7449,#7450));
#7520=DERIVED_UNIT((#7451,#7452));
#7521=DERIVED_UNIT((#7453,#7454));
#7522=DERIVED_UNIT((#7455,#7456));
#7523=DERIVED_UNIT((#7457,#7458));
#7524=DERIVED_UNIT((#7459,#7460));
#7525=DERIVED_UNIT((#7461,#7462));
#7526=DERIVED_UNIT((#7463,#7464));
#7527=DERIVED_UNIT((#7465,#7466));
#7528=DERIVED_UNIT((#7467,#7468));
#7529=DERIVED_UNIT((#7469,#7470));
#7530=DERIVED_UNIT((#7471,#7472));
#7531=DERIVED_UNIT((#7473,#7474));
#7532=DERIVED_UNIT((#7475,#7476));
#7533=DERIVED_UNIT((#7477,#7478));
#7534=DERIVED_UNIT((#7479,#7480));
#7535=DERIVED_UNIT((#7481,#7482));
#7536=DERIVED_UNIT((#7483,#7484));
#7537=DERIVED_UNIT((#7485,#7486));
#7538=MEASURE_REPRESENTATION_ITEM('density measure',
POSITIVE_RATIO_MEASURE(7850.),#7488);
#7539=MEASURE_REPRESENTATION_ITEM('density measure',
POSITIVE_RATIO_MEASURE(7850.),#7489);
#7540=MEASURE_REPRESENTATION_ITEM('density measure',
POSITIVE_RATIO_MEASURE(7850.),#7490);
#7541=MEASURE_REPRESENTATION_ITEM('density measure',
POSITIVE_RATIO_MEASURE(7850.),#7491);
#7542=MEASURE_REPRESENTATION_ITEM('density measure',
POSITIVE_RATIO_MEASURE(7850.),#7492);
#7543=MEASURE_REPRESENTATION_ITEM('density measure',
POSITIVE_RATIO_MEASURE(7850.),#7493);
#7544=MEASURE_REPRESENTATION_ITEM('density measure',
POSITIVE_RATIO_MEASURE(7850.),#7494);
#7545=MEASURE_REPRESENTATION_ITEM('density measure',
POSITIVE_RATIO_MEASURE(7850.),#7495);
#7546=MEASURE_REPRESENTATION_ITEM('density measure',
POSITIVE_RATIO_MEASURE(7850.),#7496);
#7547=MEASURE_REPRESENTATION_ITEM('density measure',
POSITIVE_RATIO_MEASURE(7850.),#7497);
#7548=MEASURE_REPRESENTATION_ITEM('density measure',
POSITIVE_RATIO_MEASURE(7850.),#7498);
#7549=MEASURE_REPRESENTATION_ITEM('density measure',
POSITIVE_RATIO_MEASURE(7850.),#7499);
#7550=MEASURE_REPRESENTATION_ITEM('density measure',
POSITIVE_RATIO_MEASURE(7850.),#7500);
#7551=MEASURE_REPRESENTATION_ITEM('density measure',
POSITIVE_RATIO_MEASURE(7850.),#7501);
#7552=MEASURE_REPRESENTATION_ITEM('density measure',
POSITIVE_RATIO_MEASURE(7850.),#7502);
#7553=MEASURE_REPRESENTATION_ITEM('density measure',
POSITIVE_RATIO_MEASURE(7850.),#7503);
#7554=MEASURE_REPRESENTATION_ITEM('density measure',
POSITIVE_RATIO_MEASURE(7850.),#7504);
#7555=MEASURE_REPRESENTATION_ITEM('density measure',
POSITIVE_RATIO_MEASURE(7850.),#7505);
#7556=MEASURE_REPRESENTATION_ITEM('density measure',
POSITIVE_RATIO_MEASURE(7850.),#7506);
#7557=MEASURE_REPRESENTATION_ITEM('density measure',
POSITIVE_RATIO_MEASURE(7850.),#7507);
#7558=MEASURE_REPRESENTATION_ITEM('density measure',
POSITIVE_RATIO_MEASURE(7850.),#7508);
#7559=MEASURE_REPRESENTATION_ITEM('density measure',
POSITIVE_RATIO_MEASURE(7850.),#7509);
#7560=MEASURE_REPRESENTATION_ITEM('density measure',
POSITIVE_RATIO_MEASURE(7850.),#7510);
#7561=MEASURE_REPRESENTATION_ITEM('density measure',
POSITIVE_RATIO_MEASURE(7850.),#7511);
#7562=MEASURE_REPRESENTATION_ITEM('density measure',
POSITIVE_RATIO_MEASURE(7850.),#7512);
#7563=MEASURE_REPRESENTATION_ITEM('density measure',
POSITIVE_RATIO_MEASURE(7850.),#7513);
#7564=MEASURE_REPRESENTATION_ITEM('density measure',
POSITIVE_RATIO_MEASURE(7850.),#7514);
#7565=MEASURE_REPRESENTATION_ITEM('density measure',
POSITIVE_RATIO_MEASURE(7850.),#7515);
#7566=MEASURE_REPRESENTATION_ITEM('density measure',
POSITIVE_RATIO_MEASURE(7850.),#7516);
#7567=MEASURE_REPRESENTATION_ITEM('density measure',
POSITIVE_RATIO_MEASURE(7850.),#7517);
#7568=MEASURE_REPRESENTATION_ITEM('density measure',
POSITIVE_RATIO_MEASURE(7850.),#7518);
#7569=MEASURE_REPRESENTATION_ITEM('density measure',
POSITIVE_RATIO_MEASURE(7850.),#7519);
#7570=MEASURE_REPRESENTATION_ITEM('density measure',
POSITIVE_RATIO_MEASURE(7850.),#7520);
#7571=MEASURE_REPRESENTATION_ITEM('density measure',
POSITIVE_RATIO_MEASURE(7850.),#7521);
#7572=MEASURE_REPRESENTATION_ITEM('density measure',
POSITIVE_RATIO_MEASURE(7850.),#7522);
#7573=MEASURE_REPRESENTATION_ITEM('density measure',
POSITIVE_RATIO_MEASURE(7850.),#7523);
#7574=MEASURE_REPRESENTATION_ITEM('density measure',
POSITIVE_RATIO_MEASURE(7850.),#7524);
#7575=MEASURE_REPRESENTATION_ITEM('density measure',
POSITIVE_RATIO_MEASURE(7850.),#7525);
#7576=MEASURE_REPRESENTATION_ITEM('density measure',
POSITIVE_RATIO_MEASURE(7850.),#7526);
#7577=MEASURE_REPRESENTATION_ITEM('density measure',
POSITIVE_RATIO_MEASURE(7850.),#7527);
#7578=MEASURE_REPRESENTATION_ITEM('density measure',
POSITIVE_RATIO_MEASURE(7850.),#7528);
#7579=MEASURE_REPRESENTATION_ITEM('density measure',
POSITIVE_RATIO_MEASURE(7850.),#7529);
#7580=MEASURE_REPRESENTATION_ITEM('density measure',
POSITIVE_RATIO_MEASURE(7850.),#7530);
#7581=MEASURE_REPRESENTATION_ITEM('density measure',
POSITIVE_RATIO_MEASURE(7850.),#7531);
#7582=MEASURE_REPRESENTATION_ITEM('density measure',
POSITIVE_RATIO_MEASURE(7850.),#7532);
#7583=MEASURE_REPRESENTATION_ITEM('density measure',
POSITIVE_RATIO_MEASURE(7850.),#7533);
#7584=MEASURE_REPRESENTATION_ITEM('density measure',
POSITIVE_RATIO_MEASURE(7850.),#7534);
#7585=MEASURE_REPRESENTATION_ITEM('density measure',
POSITIVE_RATIO_MEASURE(7850.),#7535);
#7586=MEASURE_REPRESENTATION_ITEM('density measure',
POSITIVE_RATIO_MEASURE(7850.),#7536);
#7587=MEASURE_REPRESENTATION_ITEM('density measure',
POSITIVE_RATIO_MEASURE(7850.),#7537);
#7588=PROPERTY_DEFINITION_REPRESENTATION(#7838,#7688);
#7589=PROPERTY_DEFINITION_REPRESENTATION(#7839,#7689);
#7590=PROPERTY_DEFINITION_REPRESENTATION(#7840,#7690);
#7591=PROPERTY_DEFINITION_REPRESENTATION(#7841,#7691);
#7592=PROPERTY_DEFINITION_REPRESENTATION(#7842,#7692);
#7593=PROPERTY_DEFINITION_REPRESENTATION(#7843,#7693);
#7594=PROPERTY_DEFINITION_REPRESENTATION(#7844,#7694);
#7595=PROPERTY_DEFINITION_REPRESENTATION(#7845,#7695);
#7596=PROPERTY_DEFINITION_REPRESENTATION(#7846,#7696);
#7597=PROPERTY_DEFINITION_REPRESENTATION(#7847,#7697);
#7598=PROPERTY_DEFINITION_REPRESENTATION(#7848,#7698);
#7599=PROPERTY_DEFINITION_REPRESENTATION(#7849,#7699);
#7600=PROPERTY_DEFINITION_REPRESENTATION(#7850,#7700);
#7601=PROPERTY_DEFINITION_REPRESENTATION(#7851,#7701);
#7602=PROPERTY_DEFINITION_REPRESENTATION(#7852,#7702);
#7603=PROPERTY_DEFINITION_REPRESENTATION(#7853,#7703);
#7604=PROPERTY_DEFINITION_REPRESENTATION(#7854,#7704);
#7605=PROPERTY_DEFINITION_REPRESENTATION(#7855,#7705);
#7606=PROPERTY_DEFINITION_REPRESENTATION(#7856,#7706);
#7607=PROPERTY_DEFINITION_REPRESENTATION(#7857,#7707);
#7608=PROPERTY_DEFINITION_REPRESENTATION(#7858,#7708);
#7609=PROPERTY_DEFINITION_REPRESENTATION(#7859,#7709);
#7610=PROPERTY_DEFINITION_REPRESENTATION(#7860,#7710);
#7611=PROPERTY_DEFINITION_REPRESENTATION(#7861,#7711);
#7612=PROPERTY_DEFINITION_REPRESENTATION(#7862,#7712);
#7613=PROPERTY_DEFINITION_REPRESENTATION(#7863,#7713);
#7614=PROPERTY_DEFINITION_REPRESENTATION(#7864,#7714);
#7615=PROPERTY_DEFINITION_REPRESENTATION(#7865,#7715);
#7616=PROPERTY_DEFINITION_REPRESENTATION(#7866,#7716);
#7617=PROPERTY_DEFINITION_REPRESENTATION(#7867,#7717);
#7618=PROPERTY_DEFINITION_REPRESENTATION(#7868,#7718);
#7619=PROPERTY_DEFINITION_REPRESENTATION(#7869,#7719);
#7620=PROPERTY_DEFINITION_REPRESENTATION(#7870,#7720);
#7621=PROPERTY_DEFINITION_REPRESENTATION(#7871,#7721);
#7622=PROPERTY_DEFINITION_REPRESENTATION(#7872,#7722);
#7623=PROPERTY_DEFINITION_REPRESENTATION(#7873,#7723);
#7624=PROPERTY_DEFINITION_REPRESENTATION(#7874,#7724);
#7625=PROPERTY_DEFINITION_REPRESENTATION(#7875,#7725);
#7626=PROPERTY_DEFINITION_REPRESENTATION(#7876,#7726);
#7627=PROPERTY_DEFINITION_REPRESENTATION(#7877,#7727);
#7628=PROPERTY_DEFINITION_REPRESENTATION(#7878,#7728);
#7629=PROPERTY_DEFINITION_REPRESENTATION(#7879,#7729);
#7630=PROPERTY_DEFINITION_REPRESENTATION(#7880,#7730);
#7631=PROPERTY_DEFINITION_REPRESENTATION(#7881,#7731);
#7632=PROPERTY_DEFINITION_REPRESENTATION(#7882,#7732);
#7633=PROPERTY_DEFINITION_REPRESENTATION(#7883,#7733);
#7634=PROPERTY_DEFINITION_REPRESENTATION(#7884,#7734);
#7635=PROPERTY_DEFINITION_REPRESENTATION(#7885,#7735);
#7636=PROPERTY_DEFINITION_REPRESENTATION(#7886,#7736);
#7637=PROPERTY_DEFINITION_REPRESENTATION(#7887,#7737);
#7638=PROPERTY_DEFINITION_REPRESENTATION(#7888,#7738);
#7639=PROPERTY_DEFINITION_REPRESENTATION(#7889,#7739);
#7640=PROPERTY_DEFINITION_REPRESENTATION(#7890,#7740);
#7641=PROPERTY_DEFINITION_REPRESENTATION(#7891,#7741);
#7642=PROPERTY_DEFINITION_REPRESENTATION(#7892,#7742);
#7643=PROPERTY_DEFINITION_REPRESENTATION(#7893,#7743);
#7644=PROPERTY_DEFINITION_REPRESENTATION(#7894,#7744);
#7645=PROPERTY_DEFINITION_REPRESENTATION(#7895,#7745);
#7646=PROPERTY_DEFINITION_REPRESENTATION(#7896,#7746);
#7647=PROPERTY_DEFINITION_REPRESENTATION(#7897,#7747);
#7648=PROPERTY_DEFINITION_REPRESENTATION(#7898,#7748);
#7649=PROPERTY_DEFINITION_REPRESENTATION(#7899,#7749);
#7650=PROPERTY_DEFINITION_REPRESENTATION(#7900,#7750);
#7651=PROPERTY_DEFINITION_REPRESENTATION(#7901,#7751);
#7652=PROPERTY_DEFINITION_REPRESENTATION(#7902,#7752);
#7653=PROPERTY_DEFINITION_REPRESENTATION(#7903,#7753);
#7654=PROPERTY_DEFINITION_REPRESENTATION(#7904,#7754);
#7655=PROPERTY_DEFINITION_REPRESENTATION(#7905,#7755);
#7656=PROPERTY_DEFINITION_REPRESENTATION(#7906,#7756);
#7657=PROPERTY_DEFINITION_REPRESENTATION(#7907,#7757);
#7658=PROPERTY_DEFINITION_REPRESENTATION(#7908,#7758);
#7659=PROPERTY_DEFINITION_REPRESENTATION(#7909,#7759);
#7660=PROPERTY_DEFINITION_REPRESENTATION(#7910,#7760);
#7661=PROPERTY_DEFINITION_REPRESENTATION(#7911,#7761);
#7662=PROPERTY_DEFINITION_REPRESENTATION(#7912,#7762);
#7663=PROPERTY_DEFINITION_REPRESENTATION(#7913,#7763);
#7664=PROPERTY_DEFINITION_REPRESENTATION(#7914,#7764);
#7665=PROPERTY_DEFINITION_REPRESENTATION(#7915,#7765);
#7666=PROPERTY_DEFINITION_REPRESENTATION(#7916,#7766);
#7667=PROPERTY_DEFINITION_REPRESENTATION(#7917,#7767);
#7668=PROPERTY_DEFINITION_REPRESENTATION(#7918,#7768);
#7669=PROPERTY_DEFINITION_REPRESENTATION(#7919,#7769);
#7670=PROPERTY_DEFINITION_REPRESENTATION(#7920,#7770);
#7671=PROPERTY_DEFINITION_REPRESENTATION(#7921,#7771);
#7672=PROPERTY_DEFINITION_REPRESENTATION(#7922,#7772);
#7673=PROPERTY_DEFINITION_REPRESENTATION(#7923,#7773);
#7674=PROPERTY_DEFINITION_REPRESENTATION(#7924,#7774);
#7675=PROPERTY_DEFINITION_REPRESENTATION(#7925,#7775);
#7676=PROPERTY_DEFINITION_REPRESENTATION(#7926,#7776);
#7677=PROPERTY_DEFINITION_REPRESENTATION(#7927,#7777);
#7678=PROPERTY_DEFINITION_REPRESENTATION(#7928,#7778);
#7679=PROPERTY_DEFINITION_REPRESENTATION(#7929,#7779);
#7680=PROPERTY_DEFINITION_REPRESENTATION(#7930,#7780);
#7681=PROPERTY_DEFINITION_REPRESENTATION(#7931,#7781);
#7682=PROPERTY_DEFINITION_REPRESENTATION(#7932,#7782);
#7683=PROPERTY_DEFINITION_REPRESENTATION(#7933,#7783);
#7684=PROPERTY_DEFINITION_REPRESENTATION(#7934,#7784);
#7685=PROPERTY_DEFINITION_REPRESENTATION(#7935,#7785);
#7686=PROPERTY_DEFINITION_REPRESENTATION(#7936,#7786);
#7687=PROPERTY_DEFINITION_REPRESENTATION(#7937,#7787);
#7688=REPRESENTATION('material name',(#7788),#14458);
#7689=REPRESENTATION('density',(#7538),#14458);
#7690=REPRESENTATION('material name',(#7789),#14459);
#7691=REPRESENTATION('density',(#7539),#14459);
#7692=REPRESENTATION('material name',(#7790),#14460);
#7693=REPRESENTATION('density',(#7540),#14460);
#7694=REPRESENTATION('material name',(#7791),#14461);
#7695=REPRESENTATION('density',(#7541),#14461);
#7696=REPRESENTATION('material name',(#7792),#14462);
#7697=REPRESENTATION('density',(#7542),#14462);
#7698=REPRESENTATION('material name',(#7793),#14463);
#7699=REPRESENTATION('density',(#7543),#14463);
#7700=REPRESENTATION('material name',(#7794),#14464);
#7701=REPRESENTATION('density',(#7544),#14464);
#7702=REPRESENTATION('material name',(#7795),#14465);
#7703=REPRESENTATION('density',(#7545),#14465);
#7704=REPRESENTATION('material name',(#7796),#14466);
#7705=REPRESENTATION('density',(#7546),#14466);
#7706=REPRESENTATION('material name',(#7797),#14467);
#7707=REPRESENTATION('density',(#7547),#14467);
#7708=REPRESENTATION('material name',(#7798),#14468);
#7709=REPRESENTATION('density',(#7548),#14468);
#7710=REPRESENTATION('material name',(#7799),#14469);
#7711=REPRESENTATION('density',(#7549),#14469);
#7712=REPRESENTATION('material name',(#7800),#14470);
#7713=REPRESENTATION('density',(#7550),#14470);
#7714=REPRESENTATION('material name',(#7801),#14471);
#7715=REPRESENTATION('density',(#7551),#14471);
#7716=REPRESENTATION('material name',(#7802),#14472);
#7717=REPRESENTATION('density',(#7552),#14472);
#7718=REPRESENTATION('material name',(#7803),#14473);
#7719=REPRESENTATION('density',(#7553),#14473);
#7720=REPRESENTATION('material name',(#7804),#14474);
#7721=REPRESENTATION('density',(#7554),#14474);
#7722=REPRESENTATION('material name',(#7805),#14476);
#7723=REPRESENTATION('density',(#7555),#14476);
#7724=REPRESENTATION('material name',(#7806),#14477);
#7725=REPRESENTATION('density',(#7556),#14477);
#7726=REPRESENTATION('material name',(#7807),#14478);
#7727=REPRESENTATION('density',(#7557),#14478);
#7728=REPRESENTATION('material name',(#7808),#14479);
#7729=REPRESENTATION('density',(#7558),#14479);
#7730=REPRESENTATION('material name',(#7809),#14480);
#7731=REPRESENTATION('density',(#7559),#14480);
#7732=REPRESENTATION('material name',(#7810),#14481);
#7733=REPRESENTATION('density',(#7560),#14481);
#7734=REPRESENTATION('material name',(#7811),#14482);
#7735=REPRESENTATION('density',(#7561),#14482);
#7736=REPRESENTATION('material name',(#7812),#14483);
#7737=REPRESENTATION('density',(#7562),#14483);
#7738=REPRESENTATION('material name',(#7813),#14485);
#7739=REPRESENTATION('density',(#7563),#14485);
#7740=REPRESENTATION('material name',(#7814),#14486);
#7741=REPRESENTATION('density',(#7564),#14486);
#7742=REPRESENTATION('material name',(#7815),#14487);
#7743=REPRESENTATION('density',(#7565),#14487);
#7744=REPRESENTATION('material name',(#7816),#14488);
#7745=REPRESENTATION('density',(#7566),#14488);
#7746=REPRESENTATION('material name',(#7817),#14489);
#7747=REPRESENTATION('density',(#7567),#14489);
#7748=REPRESENTATION('material name',(#7818),#14490);
#7749=REPRESENTATION('density',(#7568),#14490);
#7750=REPRESENTATION('material name',(#7819),#14491);
#7751=REPRESENTATION('density',(#7569),#14491);
#7752=REPRESENTATION('material name',(#7820),#14493);
#7753=REPRESENTATION('density',(#7570),#14493);
#7754=REPRESENTATION('material name',(#7821),#14494);
#7755=REPRESENTATION('density',(#7571),#14494);
#7756=REPRESENTATION('material name',(#7822),#14495);
#7757=REPRESENTATION('density',(#7572),#14495);
#7758=REPRESENTATION('material name',(#7823),#14496);
#7759=REPRESENTATION('density',(#7573),#14496);
#7760=REPRESENTATION('material name',(#7824),#14497);
#7761=REPRESENTATION('density',(#7574),#14497);
#7762=REPRESENTATION('material name',(#7825),#14498);
#7763=REPRESENTATION('density',(#7575),#14498);
#7764=REPRESENTATION('material name',(#7826),#14500);
#7765=REPRESENTATION('density',(#7576),#14500);
#7766=REPRESENTATION('material name',(#7827),#14501);
#7767=REPRESENTATION('density',(#7577),#14501);
#7768=REPRESENTATION('material name',(#7828),#14502);
#7769=REPRESENTATION('density',(#7578),#14502);
#7770=REPRESENTATION('material name',(#7829),#14503);
#7771=REPRESENTATION('density',(#7579),#14503);
#7772=REPRESENTATION('material name',(#7830),#14504);
#7773=REPRESENTATION('density',(#7580),#14504);
#7774=REPRESENTATION('material name',(#7831),#14505);
#7775=REPRESENTATION('density',(#7581),#14505);
#7776=REPRESENTATION('material name',(#7832),#14506);
#7777=REPRESENTATION('density',(#7582),#14506);
#7778=REPRESENTATION('material name',(#7833),#14507);
#7779=REPRESENTATION('density',(#7583),#14507);
#7780=REPRESENTATION('material name',(#7834),#14508);
#7781=REPRESENTATION('density',(#7584),#14508);
#7782=REPRESENTATION('material name',(#7835),#14509);
#7783=REPRESENTATION('density',(#7585),#14509);
#7784=REPRESENTATION('material name',(#7836),#14510);
#7785=REPRESENTATION('density',(#7586),#14510);
#7786=REPRESENTATION('material name',(#7837),#14511);
#7787=REPRESENTATION('density',(#7587),#14511);
#7788=DESCRIPTIVE_REPRESENTATION_ITEM('Steel','Steel');
#7789=DESCRIPTIVE_REPRESENTATION_ITEM('Steel','Steel');
#7790=DESCRIPTIVE_REPRESENTATION_ITEM('Steel','Steel');
#7791=DESCRIPTIVE_REPRESENTATION_ITEM('Steel','Steel');
#7792=DESCRIPTIVE_REPRESENTATION_ITEM('Steel','Steel');
#7793=DESCRIPTIVE_REPRESENTATION_ITEM('Steel','Steel');
#7794=DESCRIPTIVE_REPRESENTATION_ITEM('Steel','Steel');
#7795=DESCRIPTIVE_REPRESENTATION_ITEM('Steel','Steel');
#7796=DESCRIPTIVE_REPRESENTATION_ITEM('Steel','Steel');
#7797=DESCRIPTIVE_REPRESENTATION_ITEM('Steel','Steel');
#7798=DESCRIPTIVE_REPRESENTATION_ITEM('Steel','Steel');
#7799=DESCRIPTIVE_REPRESENTATION_ITEM('Steel','Steel');
#7800=DESCRIPTIVE_REPRESENTATION_ITEM('Steel','Steel');
#7801=DESCRIPTIVE_REPRESENTATION_ITEM('Steel','Steel');
#7802=DESCRIPTIVE_REPRESENTATION_ITEM('Steel','Steel');
#7803=DESCRIPTIVE_REPRESENTATION_ITEM('Steel','Steel');
#7804=DESCRIPTIVE_REPRESENTATION_ITEM('Steel','Steel');
#7805=DESCRIPTIVE_REPRESENTATION_ITEM('Steel','Steel');
#7806=DESCRIPTIVE_REPRESENTATION_ITEM('Steel','Steel');
#7807=DESCRIPTIVE_REPRESENTATION_ITEM('Steel','Steel');
#7808=DESCRIPTIVE_REPRESENTATION_ITEM('Steel','Steel');
#7809=DESCRIPTIVE_REPRESENTATION_ITEM('Steel','Steel');
#7810=DESCRIPTIVE_REPRESENTATION_ITEM('Steel','Steel');
#7811=DESCRIPTIVE_REPRESENTATION_ITEM('Steel','Steel');
#7812=DESCRIPTIVE_REPRESENTATION_ITEM('Steel','Steel');
#7813=DESCRIPTIVE_REPRESENTATION_ITEM('Steel','Steel');
#7814=DESCRIPTIVE_REPRESENTATION_ITEM('Steel','Steel');
#7815=DESCRIPTIVE_REPRESENTATION_ITEM('Steel','Steel');
#7816=DESCRIPTIVE_REPRESENTATION_ITEM('Steel','Steel');
#7817=DESCRIPTIVE_REPRESENTATION_ITEM('Steel','Steel');
#7818=DESCRIPTIVE_REPRESENTATION_ITEM('Steel','Steel');
#7819=DESCRIPTIVE_REPRESENTATION_ITEM('Steel','Steel');
#7820=DESCRIPTIVE_REPRESENTATION_ITEM('Steel','Steel');
#7821=DESCRIPTIVE_REPRESENTATION_ITEM('Steel','Steel');
#7822=DESCRIPTIVE_REPRESENTATION_ITEM('Steel','Steel');
#7823=DESCRIPTIVE_REPRESENTATION_ITEM('Steel','Steel');
#7824=DESCRIPTIVE_REPRESENTATION_ITEM('Steel','Steel');
#7825=DESCRIPTIVE_REPRESENTATION_ITEM('Steel','Steel');
#7826=DESCRIPTIVE_REPRESENTATION_ITEM('Steel','Steel');
#7827=DESCRIPTIVE_REPRESENTATION_ITEM('Steel','Steel');
#7828=DESCRIPTIVE_REPRESENTATION_ITEM('Steel','Steel');
#7829=DESCRIPTIVE_REPRESENTATION_ITEM('Steel','Steel');
#7830=DESCRIPTIVE_REPRESENTATION_ITEM('Steel','Steel');
#7831=DESCRIPTIVE_REPRESENTATION_ITEM('Steel','Steel');
#7832=DESCRIPTIVE_REPRESENTATION_ITEM('Steel','Steel');
#7833=DESCRIPTIVE_REPRESENTATION_ITEM('Steel','Steel');
#7834=DESCRIPTIVE_REPRESENTATION_ITEM('Steel','Steel');
#7835=DESCRIPTIVE_REPRESENTATION_ITEM('Steel','Steel');
#7836=DESCRIPTIVE_REPRESENTATION_ITEM('Steel','Steel');
#7837=DESCRIPTIVE_REPRESENTATION_ITEM('Steel','Steel');
#7838=PROPERTY_DEFINITION('material property','material name',#14800);
#7839=PROPERTY_DEFINITION('material property','density of part',#14800);
#7840=PROPERTY_DEFINITION('material property','material name',#14801);
#7841=PROPERTY_DEFINITION('material property','density of part',#14801);
#7842=PROPERTY_DEFINITION('material property','material name',#14802);
#7843=PROPERTY_DEFINITION('material property','density of part',#14802);
#7844=PROPERTY_DEFINITION('material property','material name',#14803);
#7845=PROPERTY_DEFINITION('material property','density of part',#14803);
#7846=PROPERTY_DEFINITION('material property','material name',#14804);
#7847=PROPERTY_DEFINITION('material property','density of part',#14804);
#7848=PROPERTY_DEFINITION('material property','material name',#14805);
#7849=PROPERTY_DEFINITION('material property','density of part',#14805);
#7850=PROPERTY_DEFINITION('material property','material name',#14806);
#7851=PROPERTY_DEFINITION('material property','density of part',#14806);
#7852=PROPERTY_DEFINITION('material property','material name',#14807);
#7853=PROPERTY_DEFINITION('material property','density of part',#14807);
#7854=PROPERTY_DEFINITION('material property','material name',#14808);
#7855=PROPERTY_DEFINITION('material property','density of part',#14808);
#7856=PROPERTY_DEFINITION('material property','material name',#14809);
#7857=PROPERTY_DEFINITION('material property','density of part',#14809);
#7858=PROPERTY_DEFINITION('material property','material name',#14810);
#7859=PROPERTY_DEFINITION('material property','density of part',#14810);
#7860=PROPERTY_DEFINITION('material property','material name',#14811);
#7861=PROPERTY_DEFINITION('material property','density of part',#14811);
#7862=PROPERTY_DEFINITION('material property','material name',#14812);
#7863=PROPERTY_DEFINITION('material property','density of part',#14812);
#7864=PROPERTY_DEFINITION('material property','material name',#14813);
#7865=PROPERTY_DEFINITION('material property','density of part',#14813);
#7866=PROPERTY_DEFINITION('material property','material name',#14814);
#7867=PROPERTY_DEFINITION('material property','density of part',#14814);
#7868=PROPERTY_DEFINITION('material property','material name',#14815);
#7869=PROPERTY_DEFINITION('material property','density of part',#14815);
#7870=PROPERTY_DEFINITION('material property','material name',#14816);
#7871=PROPERTY_DEFINITION('material property','density of part',#14816);
#7872=PROPERTY_DEFINITION('material property','material name',#14818);
#7873=PROPERTY_DEFINITION('material property','density of part',#14818);
#7874=PROPERTY_DEFINITION('material property','material name',#14819);
#7875=PROPERTY_DEFINITION('material property','density of part',#14819);
#7876=PROPERTY_DEFINITION('material property','material name',#14820);
#7877=PROPERTY_DEFINITION('material property','density of part',#14820);
#7878=PROPERTY_DEFINITION('material property','material name',#14821);
#7879=PROPERTY_DEFINITION('material property','density of part',#14821);
#7880=PROPERTY_DEFINITION('material property','material name',#14822);
#7881=PROPERTY_DEFINITION('material property','density of part',#14822);
#7882=PROPERTY_DEFINITION('material property','material name',#14823);
#7883=PROPERTY_DEFINITION('material property','density of part',#14823);
#7884=PROPERTY_DEFINITION('material property','material name',#14824);
#7885=PROPERTY_DEFINITION('material property','density of part',#14824);
#7886=PROPERTY_DEFINITION('material property','material name',#14825);
#7887=PROPERTY_DEFINITION('material property','density of part',#14825);
#7888=PROPERTY_DEFINITION('material property','material name',#14827);
#7889=PROPERTY_DEFINITION('material property','density of part',#14827);
#7890=PROPERTY_DEFINITION('material property','material name',#14828);
#7891=PROPERTY_DEFINITION('material property','density of part',#14828);
#7892=PROPERTY_DEFINITION('material property','material name',#14829);
#7893=PROPERTY_DEFINITION('material property','density of part',#14829);
#7894=PROPERTY_DEFINITION('material property','material name',#14830);
#7895=PROPERTY_DEFINITION('material property','density of part',#14830);
#7896=PROPERTY_DEFINITION('material property','material name',#14831);
#7897=PROPERTY_DEFINITION('material property','density of part',#14831);
#7898=PROPERTY_DEFINITION('material property','material name',#14832);
#7899=PROPERTY_DEFINITION('material property','density of part',#14832);
#7900=PROPERTY_DEFINITION('material property','material name',#14833);
#7901=PROPERTY_DEFINITION('material property','density of part',#14833);
#7902=PROPERTY_DEFINITION('material property','material name',#14835);
#7903=PROPERTY_DEFINITION('material property','density of part',#14835);
#7904=PROPERTY_DEFINITION('material property','material name',#14836);
#7905=PROPERTY_DEFINITION('material property','density of part',#14836);
#7906=PROPERTY_DEFINITION('material property','material name',#14837);
#7907=PROPERTY_DEFINITION('material property','density of part',#14837);
#7908=PROPERTY_DEFINITION('material property','material name',#14838);
#7909=PROPERTY_DEFINITION('material property','density of part',#14838);
#7910=PROPERTY_DEFINITION('material property','material name',#14839);
#7911=PROPERTY_DEFINITION('material property','density of part',#14839);
#7912=PROPERTY_DEFINITION('material property','material name',#14840);
#7913=PROPERTY_DEFINITION('material property','density of part',#14840);
#7914=PROPERTY_DEFINITION('material property','material name',#14842);
#7915=PROPERTY_DEFINITION('material property','density of part',#14842);
#7916=PROPERTY_DEFINITION('material property','material name',#14843);
#7917=PROPERTY_DEFINITION('material property','density of part',#14843);
#7918=PROPERTY_DEFINITION('material property','material name',#14844);
#7919=PROPERTY_DEFINITION('material property','density of part',#14844);
#7920=PROPERTY_DEFINITION('material property','material name',#14845);
#7921=PROPERTY_DEFINITION('material property','density of part',#14845);
#7922=PROPERTY_DEFINITION('material property','material name',#14846);
#7923=PROPERTY_DEFINITION('material property','density of part',#14846);
#7924=PROPERTY_DEFINITION('material property','material name',#14847);
#7925=PROPERTY_DEFINITION('material property','density of part',#14847);
#7926=PROPERTY_DEFINITION('material property','material name',#14848);
#7927=PROPERTY_DEFINITION('material property','density of part',#14848);
#7928=PROPERTY_DEFINITION('material property','material name',#14849);
#7929=PROPERTY_DEFINITION('material property','density of part',#14849);
#7930=PROPERTY_DEFINITION('material property','material name',#14850);
#7931=PROPERTY_DEFINITION('material property','density of part',#14850);
#7932=PROPERTY_DEFINITION('material property','material name',#14851);
#7933=PROPERTY_DEFINITION('material property','density of part',#14851);
#7934=PROPERTY_DEFINITION('material property','material name',#14852);
#7935=PROPERTY_DEFINITION('material property','density of part',#14852);
#7936=PROPERTY_DEFINITION('material property','material name',#14853);
#7937=PROPERTY_DEFINITION('material property','density of part',#14853);
#7938=AXIS2_PLACEMENT_3D('',#11428,#8970,#8971);
#7939=AXIS2_PLACEMENT_3D('',#11429,#8972,#8973);
#7940=AXIS2_PLACEMENT_3D('',#11430,#8974,#8975);
#7941=AXIS2_PLACEMENT_3D('',#11431,#8976,#8977);
#7942=AXIS2_PLACEMENT_3D('',#11433,#8978,#8979);
#7943=AXIS2_PLACEMENT_3D('',#11436,#8981,#8982);
#7944=AXIS2_PLACEMENT_3D('',#11437,#8983,#8984);
#7945=AXIS2_PLACEMENT_3D('',#11439,#8985,#8986);
#7946=AXIS2_PLACEMENT_3D('',#11442,#8988,#8989);
#7947=AXIS2_PLACEMENT_3D('',#11443,#8990,#8991);
#7948=AXIS2_PLACEMENT_3D('',#11445,#8992,#8993);
#7949=AXIS2_PLACEMENT_3D('',#11448,#8995,#8996);
#7950=AXIS2_PLACEMENT_3D('',#11449,#8997,#8998);
#7951=AXIS2_PLACEMENT_3D('',#11451,#8999,#9000);
#7952=AXIS2_PLACEMENT_3D('',#11454,#9002,#9003);
#7953=AXIS2_PLACEMENT_3D('',#11455,#9004,#9005);
#7954=AXIS2_PLACEMENT_3D('',#11464,#9010,#9011);
#7955=AXIS2_PLACEMENT_3D('',#11470,#9015,#9016);
#7956=AXIS2_PLACEMENT_3D('',#11476,#9020,#9021);
#7957=AXIS2_PLACEMENT_3D('',#11479,#9024,#9025);
#7958=AXIS2_PLACEMENT_3D('',#11480,#9026,#9027);
#7959=AXIS2_PLACEMENT_3D('',#11481,#9028,#9029);
#7960=AXIS2_PLACEMENT_3D('',#11482,#9030,#9031);
#7961=AXIS2_PLACEMENT_3D('',#11491,#9036,#9037);
#7962=AXIS2_PLACEMENT_3D('',#11497,#9041,#9042);
#7963=AXIS2_PLACEMENT_3D('',#11503,#9046,#9047);
#7964=AXIS2_PLACEMENT_3D('',#11506,#9050,#9051);
#7965=AXIS2_PLACEMENT_3D('',#11507,#9052,#9053);
#7966=AXIS2_PLACEMENT_3D('',#11508,#9054,#9055);
#7967=AXIS2_PLACEMENT_3D('',#11509,#9056,#9057);
#7968=AXIS2_PLACEMENT_3D('',#11518,#9062,#9063);
#7969=AXIS2_PLACEMENT_3D('',#11524,#9067,#9068);
#7970=AXIS2_PLACEMENT_3D('',#11530,#9072,#9073);
#7971=AXIS2_PLACEMENT_3D('',#11533,#9076,#9077);
#7972=AXIS2_PLACEMENT_3D('',#11534,#9078,#9079);
#7973=AXIS2_PLACEMENT_3D('',#11535,#9080,#9081);
#7974=AXIS2_PLACEMENT_3D('',#11536,#9082,#9083);
#7975=AXIS2_PLACEMENT_3D('',#11538,#9084,#9085);
#7976=AXIS2_PLACEMENT_3D('',#11541,#9087,#9088);
#7977=AXIS2_PLACEMENT_3D('',#11542,#9089,#9090);
#7978=AXIS2_PLACEMENT_3D('',#11543,#9091,#9092);
#7979=AXIS2_PLACEMENT_3D('',#11545,#9093,#9094);
#7980=AXIS2_PLACEMENT_3D('',#11548,#9096,#9097);
#7981=AXIS2_PLACEMENT_3D('',#11549,#9098,#9099);
#7982=AXIS2_PLACEMENT_3D('',#11551,#9100,#9101);
#7983=AXIS2_PLACEMENT_3D('',#11554,#9103,#9104);
#7984=AXIS2_PLACEMENT_3D('',#11555,#9105,#9106);
#7985=AXIS2_PLACEMENT_3D('',#11557,#9107,#9108);
#7986=AXIS2_PLACEMENT_3D('',#11560,#9110,#9111);
#7987=AXIS2_PLACEMENT_3D('',#11561,#9112,#9113);
#7988=AXIS2_PLACEMENT_3D('',#11563,#9114,#9115);
#7989=AXIS2_PLACEMENT_3D('',#11566,#9117,#9118);
#7990=AXIS2_PLACEMENT_3D('',#11567,#9119,#9120);
#7991=AXIS2_PLACEMENT_3D('',#11569,#9121,#9122);
#7992=AXIS2_PLACEMENT_3D('',#11572,#9124,#9125);
#7993=AXIS2_PLACEMENT_3D('',#11573,#9126,#9127);
#7994=AXIS2_PLACEMENT_3D('',#11575,#9128,#9129);
#7995=AXIS2_PLACEMENT_3D('',#11578,#9131,#9132);
#7996=AXIS2_PLACEMENT_3D('',#11579,#9133,#9134);
#7997=AXIS2_PLACEMENT_3D('',#11581,#9135,#9136);
#7998=AXIS2_PLACEMENT_3D('',#11584,#9138,#9139);
#7999=AXIS2_PLACEMENT_3D('',#11585,#9140,#9141);
#8000=AXIS2_PLACEMENT_3D('',#11587,#9142,#9143);
#8001=AXIS2_PLACEMENT_3D('',#11590,#9145,#9146);
#8002=AXIS2_PLACEMENT_3D('',#11591,#9147,#9148);
#8003=AXIS2_PLACEMENT_3D('',#11593,#9149,#9150);
#8004=AXIS2_PLACEMENT_3D('',#11596,#9152,#9153);
#8005=AXIS2_PLACEMENT_3D('',#11597,#9154,#9155);
#8006=AXIS2_PLACEMENT_3D('',#11599,#9156,#9157);
#8007=AXIS2_PLACEMENT_3D('',#11602,#9159,#9160);
#8008=AXIS2_PLACEMENT_3D('',#11603,#9161,#9162);
#8009=AXIS2_PLACEMENT_3D('',#11605,#9163,#9164);
#8010=AXIS2_PLACEMENT_3D('',#11608,#9166,#9167);
#8011=AXIS2_PLACEMENT_3D('',#11609,#9168,#9169);
#8012=AXIS2_PLACEMENT_3D('',#11611,#9170,#9171);
#8013=AXIS2_PLACEMENT_3D('',#11614,#9173,#9174);
#8014=AXIS2_PLACEMENT_3D('',#11615,#9175,#9176);
#8015=AXIS2_PLACEMENT_3D('',#11632,#9185,#9186);
#8016=AXIS2_PLACEMENT_3D('',#11638,#9190,#9191);
#8017=AXIS2_PLACEMENT_3D('',#11644,#9195,#9196);
#8018=AXIS2_PLACEMENT_3D('',#11647,#9199,#9200);
#8019=AXIS2_PLACEMENT_3D('',#11648,#9201,#9202);
#8020=AXIS2_PLACEMENT_3D('',#11654,#9206,#9207);
#8021=AXIS2_PLACEMENT_3D('',#11658,#9210,#9211);
#8022=AXIS2_PLACEMENT_3D('',#11662,#9214,#9215);
#8023=AXIS2_PLACEMENT_3D('',#11664,#9217,#9218);
#8024=AXIS2_PLACEMENT_3D('',#11665,#9219,#9220);
#8025=AXIS2_PLACEMENT_3D('',#11666,#9221,#9222);
#8026=AXIS2_PLACEMENT_3D('',#11668,#9223,#9224);
#8027=AXIS2_PLACEMENT_3D('',#11671,#9226,#9227);
#8028=AXIS2_PLACEMENT_3D('',#11672,#9228,#9229);
#8029=AXIS2_PLACEMENT_3D('',#11673,#9230,#9231);
#8030=AXIS2_PLACEMENT_3D('',#11675,#9232,#9233);
#8031=AXIS2_PLACEMENT_3D('',#11678,#9235,#9236);
#8032=AXIS2_PLACEMENT_3D('',#11679,#9237,#9238);
#8033=AXIS2_PLACEMENT_3D('',#11681,#9239,#9240);
#8034=AXIS2_PLACEMENT_3D('',#11684,#9242,#9243);
#8035=AXIS2_PLACEMENT_3D('',#11685,#9244,#9245);
#8036=AXIS2_PLACEMENT_3D('',#11687,#9246,#9247);
#8037=AXIS2_PLACEMENT_3D('',#11690,#9249,#9250);
#8038=AXIS2_PLACEMENT_3D('',#11691,#9251,#9252);
#8039=AXIS2_PLACEMENT_3D('',#11693,#9253,#9254);
#8040=AXIS2_PLACEMENT_3D('',#11695,#9255,#9256);
#8041=AXIS2_PLACEMENT_3D('',#11696,#9257,#9258);
#8042=AXIS2_PLACEMENT_3D('',#11698,#9259,#9260);
#8043=AXIS2_PLACEMENT_3D('',#11700,#9261,#9262);
#8044=AXIS2_PLACEMENT_3D('',#11701,#9263,#9264);
#8045=AXIS2_PLACEMENT_3D('',#11703,#9266,#9267);
#8046=AXIS2_PLACEMENT_3D('',#11706,#9269,#9270);
#8047=AXIS2_PLACEMENT_3D('',#11707,#9271,#9272);
#8048=AXIS2_PLACEMENT_3D('',#11709,#9273,#9274);
#8049=AXIS2_PLACEMENT_3D('',#11711,#9276,#9277);
#8050=AXIS2_PLACEMENT_3D('',#11712,#9278,#9279);
#8051=AXIS2_PLACEMENT_3D('',#11713,#9280,#9281);
#8052=AXIS2_PLACEMENT_3D('',#11714,#9282,#9283);
#8053=AXIS2_PLACEMENT_3D('',#11716,#9284,#9285);
#8054=AXIS2_PLACEMENT_3D('',#11719,#9287,#9288);
#8055=AXIS2_PLACEMENT_3D('',#11720,#9289,#9290);
#8056=AXIS2_PLACEMENT_3D('',#11722,#9291,#9292);
#8057=AXIS2_PLACEMENT_3D('',#11725,#9294,#9295);
#8058=AXIS2_PLACEMENT_3D('',#11726,#9296,#9297);
#8059=AXIS2_PLACEMENT_3D('',#11727,#9298,#9299);
#8060=AXIS2_PLACEMENT_3D('',#11728,#9300,#9301);
#8061=AXIS2_PLACEMENT_3D('',#11729,#9302,#9303);
#8062=AXIS2_PLACEMENT_3D('',#11731,#9304,#9305);
#8063=AXIS2_PLACEMENT_3D('',#11734,#9307,#9308);
#8064=AXIS2_PLACEMENT_3D('',#11735,#9309,#9310);
#8065=AXIS2_PLACEMENT_3D('',#11737,#9311,#9312);
#8066=AXIS2_PLACEMENT_3D('',#11740,#9314,#9315);
#8067=AXIS2_PLACEMENT_3D('',#11741,#9316,#9317);
#8068=AXIS2_PLACEMENT_3D('',#11742,#9318,#9319);
#8069=AXIS2_PLACEMENT_3D('',#11743,#9320,#9321);
#8070=AXIS2_PLACEMENT_3D('',#11744,#9322,#9323);
#8071=AXIS2_PLACEMENT_3D('',#11746,#9324,#9325);
#8072=AXIS2_PLACEMENT_3D('',#11749,#9327,#9328);
#8073=AXIS2_PLACEMENT_3D('',#11750,#9329,#9330);
#8074=AXIS2_PLACEMENT_3D('',#11752,#9331,#9332);
#8075=AXIS2_PLACEMENT_3D('',#11755,#9334,#9335);
#8076=AXIS2_PLACEMENT_3D('',#11756,#9336,#9337);
#8077=AXIS2_PLACEMENT_3D('',#11757,#9338,#9339);
#8078=AXIS2_PLACEMENT_3D('',#11758,#9340,#9341);
#8079=AXIS2_PLACEMENT_3D('',#11759,#9342,#9343);
#8080=AXIS2_PLACEMENT_3D('',#11761,#9344,#9345);
#8081=AXIS2_PLACEMENT_3D('',#11764,#9347,#9348);
#8082=AXIS2_PLACEMENT_3D('',#11765,#9349,#9350);
#8083=AXIS2_PLACEMENT_3D('',#11767,#9351,#9352);
#8084=AXIS2_PLACEMENT_3D('',#11770,#9354,#9355);
#8085=AXIS2_PLACEMENT_3D('',#11771,#9356,#9357);
#8086=AXIS2_PLACEMENT_3D('',#11772,#9358,#9359);
#8087=AXIS2_PLACEMENT_3D('',#11773,#9360,#9361);
#8088=AXIS2_PLACEMENT_3D('',#11774,#9362,#9363);
#8089=AXIS2_PLACEMENT_3D('',#11776,#9364,#9365);
#8090=AXIS2_PLACEMENT_3D('',#11779,#9367,#9368);
#8091=AXIS2_PLACEMENT_3D('',#11780,#9369,#9370);
#8092=AXIS2_PLACEMENT_3D('',#11781,#9371,#9372);
#8093=AXIS2_PLACEMENT_3D('',#11783,#9373,#9374);
#8094=AXIS2_PLACEMENT_3D('',#11786,#9376,#9377);
#8095=AXIS2_PLACEMENT_3D('',#11787,#9378,#9379);
#8096=AXIS2_PLACEMENT_3D('',#11789,#9380,#9381);
#8097=AXIS2_PLACEMENT_3D('',#11792,#9383,#9384);
#8098=AXIS2_PLACEMENT_3D('',#11793,#9385,#9386);
#8099=AXIS2_PLACEMENT_3D('',#11795,#9387,#9388);
#8100=AXIS2_PLACEMENT_3D('',#11798,#9390,#9391);
#8101=AXIS2_PLACEMENT_3D('',#11799,#9392,#9393);
#8102=AXIS2_PLACEMENT_3D('',#11801,#9394,#9395);
#8103=AXIS2_PLACEMENT_3D('',#11803,#9396,#9397);
#8104=AXIS2_PLACEMENT_3D('',#11804,#9398,#9399);
#8105=AXIS2_PLACEMENT_3D('',#11806,#9400,#9401);
#8106=AXIS2_PLACEMENT_3D('',#11808,#9402,#9403);
#8107=AXIS2_PLACEMENT_3D('',#11809,#9404,#9405);
#8108=AXIS2_PLACEMENT_3D('',#11811,#9407,#9408);
#8109=AXIS2_PLACEMENT_3D('',#11814,#9410,#9411);
#8110=AXIS2_PLACEMENT_3D('',#11815,#9412,#9413);
#8111=AXIS2_PLACEMENT_3D('',#11817,#9414,#9415);
#8112=AXIS2_PLACEMENT_3D('',#11819,#9417,#9418);
#8113=AXIS2_PLACEMENT_3D('',#11820,#9419,#9420);
#8114=AXIS2_PLACEMENT_3D('',#11821,#9421,#9422);
#8115=AXIS2_PLACEMENT_3D('',#11822,#9423,#9424);
#8116=AXIS2_PLACEMENT_3D('',#11824,#9425,#9426);
#8117=AXIS2_PLACEMENT_3D('',#11827,#9428,#9429);
#8118=AXIS2_PLACEMENT_3D('',#11828,#9430,#9431);
#8119=AXIS2_PLACEMENT_3D('',#11830,#9432,#9433);
#8120=AXIS2_PLACEMENT_3D('',#11833,#9435,#9436);
#8121=AXIS2_PLACEMENT_3D('',#11834,#9437,#9438);
#8122=AXIS2_PLACEMENT_3D('',#11835,#9439,#9440);
#8123=AXIS2_PLACEMENT_3D('',#11836,#9441,#9442);
#8124=AXIS2_PLACEMENT_3D('',#11837,#9443,#9444);
#8125=AXIS2_PLACEMENT_3D('',#11839,#9445,#9446);
#8126=AXIS2_PLACEMENT_3D('',#11842,#9448,#9449);
#8127=AXIS2_PLACEMENT_3D('',#11843,#9450,#9451);
#8128=AXIS2_PLACEMENT_3D('',#11845,#9452,#9453);
#8129=AXIS2_PLACEMENT_3D('',#11848,#9455,#9456);
#8130=AXIS2_PLACEMENT_3D('',#11849,#9457,#9458);
#8131=AXIS2_PLACEMENT_3D('',#11850,#9459,#9460);
#8132=AXIS2_PLACEMENT_3D('',#11851,#9461,#9462);
#8133=AXIS2_PLACEMENT_3D('',#11852,#9463,#9464);
#8134=AXIS2_PLACEMENT_3D('',#11854,#9465,#9466);
#8135=AXIS2_PLACEMENT_3D('',#11857,#9468,#9469);
#8136=AXIS2_PLACEMENT_3D('',#11858,#9470,#9471);
#8137=AXIS2_PLACEMENT_3D('',#11860,#9472,#9473);
#8138=AXIS2_PLACEMENT_3D('',#11863,#9475,#9476);
#8139=AXIS2_PLACEMENT_3D('',#11864,#9477,#9478);
#8140=AXIS2_PLACEMENT_3D('',#11865,#9479,#9480);
#8141=AXIS2_PLACEMENT_3D('',#11866,#9481,#9482);
#8142=AXIS2_PLACEMENT_3D('',#11867,#9483,#9484);
#8143=AXIS2_PLACEMENT_3D('',#11869,#9485,#9486);
#8144=AXIS2_PLACEMENT_3D('',#11872,#9488,#9489);
#8145=AXIS2_PLACEMENT_3D('',#11873,#9490,#9491);
#8146=AXIS2_PLACEMENT_3D('',#11875,#9492,#9493);
#8147=AXIS2_PLACEMENT_3D('',#11878,#9495,#9496);
#8148=AXIS2_PLACEMENT_3D('',#11879,#9497,#9498);
#8149=AXIS2_PLACEMENT_3D('',#11880,#9499,#9500);
#8150=AXIS2_PLACEMENT_3D('',#11881,#9501,#9502);
#8151=AXIS2_PLACEMENT_3D('',#11882,#9503,#9504);
#8152=AXIS2_PLACEMENT_3D('',#11884,#9505,#9506);
#8153=AXIS2_PLACEMENT_3D('',#11887,#9508,#9509);
#8154=AXIS2_PLACEMENT_3D('',#11888,#9510,#9511);
#8155=AXIS2_PLACEMENT_3D('',#11890,#9512,#9513);
#8156=AXIS2_PLACEMENT_3D('',#11893,#9515,#9516);
#8157=AXIS2_PLACEMENT_3D('',#11894,#9517,#9518);
#8158=AXIS2_PLACEMENT_3D('',#11903,#9523,#9524);
#8159=AXIS2_PLACEMENT_3D('',#11909,#9528,#9529);
#8160=AXIS2_PLACEMENT_3D('',#11921,#9536,#9537);
#8161=AXIS2_PLACEMENT_3D('',#11925,#9540,#9541);
#8162=AXIS2_PLACEMENT_3D('',#11931,#9545,#9546);
#8163=AXIS2_PLACEMENT_3D('',#11933,#9548,#9549);
#8164=AXIS2_PLACEMENT_3D('',#11939,#9553,#9554);
#8165=AXIS2_PLACEMENT_3D('',#11945,#9558,#9559);
#8166=AXIS2_PLACEMENT_3D('',#11948,#9562,#9563);
#8167=AXIS2_PLACEMENT_3D('',#11949,#9564,#9565);
#8168=AXIS2_PLACEMENT_3D('',#11950,#9566,#9567);
#8169=AXIS2_PLACEMENT_3D('',#11951,#9568,#9569);
#8170=AXIS2_PLACEMENT_3D('',#11953,#9570,#9571);
#8171=AXIS2_PLACEMENT_3D('',#11957,#9573,#9574);
#8172=AXIS2_PLACEMENT_3D('',#11988,#9575,#9576);
#8173=AXIS2_PLACEMENT_3D('',#11989,#9577,#9578);
#8174=AXIS2_PLACEMENT_3D('',#11990,#9579,#9580);
#8175=AXIS2_PLACEMENT_3D('',#11992,#9582,#9583);
#8176=AXIS2_PLACEMENT_3D('',#11993,#9584,#9585);
#8177=AXIS2_PLACEMENT_3D('',#11994,#9586,#9587);
#8178=AXIS2_PLACEMENT_3D('',#11996,#9588,#9589);
#8179=AXIS2_PLACEMENT_3D('',#12039,#9591,#9592);
#8180=AXIS2_PLACEMENT_3D('',#12059,#9593,#9594);
#8181=AXIS2_PLACEMENT_3D('',#12060,#9595,#9596);
#8182=AXIS2_PLACEMENT_3D('',#12062,#9598,#9599);
#8183=AXIS2_PLACEMENT_3D('',#12063,#9600,#9601);
#8184=AXIS2_PLACEMENT_3D('',#12589,#9602,#9603);
#8185=AXIS2_PLACEMENT_3D('',#12590,#9604,#9605);
#8186=AXIS2_PLACEMENT_3D('',#12599,#9610,#9611);
#8187=AXIS2_PLACEMENT_3D('',#12605,#9615,#9616);
#8188=AXIS2_PLACEMENT_3D('',#12611,#9620,#9621);
#8189=AXIS2_PLACEMENT_3D('',#12617,#9625,#9626);
#8190=AXIS2_PLACEMENT_3D('',#12623,#9630,#9631);
#8191=AXIS2_PLACEMENT_3D('',#12626,#9634,#9635);
#8192=AXIS2_PLACEMENT_3D('',#12627,#9636,#9637);
#8193=AXIS2_PLACEMENT_3D('',#12628,#9638,#9639);
#8194=AXIS2_PLACEMENT_3D('',#12630,#9640,#9641);
#8195=AXIS2_PLACEMENT_3D('',#12631,#9642,#9643);
#8196=AXIS2_PLACEMENT_3D('',#12633,#9644,#9645);
#8197=AXIS2_PLACEMENT_3D('',#12634,#9646,#9647);
#8198=AXIS2_PLACEMENT_3D('',#12636,#9648,#9649);
#8199=AXIS2_PLACEMENT_3D('',#12638,#9651,#9652);
#8200=AXIS2_PLACEMENT_3D('',#12640,#9653,#9654);
#8201=AXIS2_PLACEMENT_3D('',#12642,#9656,#9657);
#8202=AXIS2_PLACEMENT_3D('',#12644,#9658,#9659);
#8203=AXIS2_PLACEMENT_3D('',#12646,#9661,#9662);
#8204=AXIS2_PLACEMENT_3D('',#12648,#9663,#9664);
#8205=AXIS2_PLACEMENT_3D('',#12649,#9665,#9666);
#8206=AXIS2_PLACEMENT_3D('',#12651,#9667,#9668);
#8207=AXIS2_PLACEMENT_3D('',#12653,#9670,#9671);
#8208=AXIS2_PLACEMENT_3D('',#12655,#9673,#9674);
#8209=AXIS2_PLACEMENT_3D('',#12656,#9675,#9676);
#8210=AXIS2_PLACEMENT_3D('',#12657,#9677,#9678);
#8211=AXIS2_PLACEMENT_3D('',#12659,#9679,#9680);
#8212=AXIS2_PLACEMENT_3D('',#12662,#9682,#9683);
#8213=AXIS2_PLACEMENT_3D('',#12663,#9684,#9685);
#8214=AXIS2_PLACEMENT_3D('',#12665,#9686,#9687);
#8215=AXIS2_PLACEMENT_3D('',#12668,#9689,#9690);
#8216=AXIS2_PLACEMENT_3D('',#12669,#9691,#9692);
#8217=AXIS2_PLACEMENT_3D('',#12671,#9693,#9694);
#8218=AXIS2_PLACEMENT_3D('',#12674,#9696,#9697);
#8219=AXIS2_PLACEMENT_3D('',#12675,#9698,#9699);
#8220=AXIS2_PLACEMENT_3D('',#12677,#9700,#9701);
#8221=AXIS2_PLACEMENT_3D('',#12680,#9703,#9704);
#8222=AXIS2_PLACEMENT_3D('',#12681,#9705,#9706);
#8223=AXIS2_PLACEMENT_3D('',#12683,#9707,#9708);
#8224=AXIS2_PLACEMENT_3D('',#12686,#9710,#9711);
#8225=AXIS2_PLACEMENT_3D('',#12687,#9712,#9713);
#8226=AXIS2_PLACEMENT_3D('',#12689,#9714,#9715);
#8227=AXIS2_PLACEMENT_3D('',#12692,#9717,#9718);
#8228=AXIS2_PLACEMENT_3D('',#12693,#9719,#9720);
#8229=AXIS2_PLACEMENT_3D('',#12695,#9721,#9722);
#8230=AXIS2_PLACEMENT_3D('',#12698,#9724,#9725);
#8231=AXIS2_PLACEMENT_3D('',#12699,#9726,#9727);
#8232=AXIS2_PLACEMENT_3D('',#12701,#9728,#9729);
#8233=AXIS2_PLACEMENT_3D('',#12704,#9731,#9732);
#8234=AXIS2_PLACEMENT_3D('',#12705,#9733,#9734);
#8235=AXIS2_PLACEMENT_3D('',#12707,#9735,#9736);
#8236=AXIS2_PLACEMENT_3D('',#12710,#9738,#9739);
#8237=AXIS2_PLACEMENT_3D('',#12711,#9740,#9741);
#8238=AXIS2_PLACEMENT_3D('',#12713,#9742,#9743);
#8239=AXIS2_PLACEMENT_3D('',#12716,#9745,#9746);
#8240=AXIS2_PLACEMENT_3D('',#12717,#9747,#9748);
#8241=AXIS2_PLACEMENT_3D('',#12722,#9750,#9751);
#8242=AXIS2_PLACEMENT_3D('',#12725,#9753,#9754);
#8243=AXIS2_PLACEMENT_3D('',#12726,#9755,#9756);
#8244=AXIS2_PLACEMENT_3D('',#12732,#9760,#9761);
#8245=AXIS2_PLACEMENT_3D('',#12735,#9763,#9764);
#8246=AXIS2_PLACEMENT_3D('',#12736,#9765,#9766);
#8247=AXIS2_PLACEMENT_3D('',#12740,#9769,#9770);
#8248=AXIS2_PLACEMENT_3D('',#12741,#9771,#9772);
#8249=AXIS2_PLACEMENT_3D('',#12742,#9773,#9774);
#8250=AXIS2_PLACEMENT_3D('',#12743,#9775,#9776);
#8251=AXIS2_PLACEMENT_3D('',#12744,#9777,#9778);
#8252=AXIS2_PLACEMENT_3D('',#12746,#9779,#9780);
#8253=AXIS2_PLACEMENT_3D('',#12749,#9782,#9783);
#8254=AXIS2_PLACEMENT_3D('',#12750,#9784,#9785);
#8255=AXIS2_PLACEMENT_3D('',#12752,#9786,#9787);
#8256=AXIS2_PLACEMENT_3D('',#12755,#9789,#9790);
#8257=AXIS2_PLACEMENT_3D('',#12756,#9791,#9792);
#8258=AXIS2_PLACEMENT_3D('',#12757,#9793,#9794);
#8259=AXIS2_PLACEMENT_3D('',#12758,#9795,#9796);
#8260=AXIS2_PLACEMENT_3D('',#12759,#9797,#9798);
#8261=AXIS2_PLACEMENT_3D('',#12761,#9799,#9800);
#8262=AXIS2_PLACEMENT_3D('',#12764,#9802,#9803);
#8263=AXIS2_PLACEMENT_3D('',#12765,#9804,#9805);
#8264=AXIS2_PLACEMENT_3D('',#12767,#9806,#9807);
#8265=AXIS2_PLACEMENT_3D('',#12770,#9809,#9810);
#8266=AXIS2_PLACEMENT_3D('',#12771,#9811,#9812);
#8267=AXIS2_PLACEMENT_3D('',#12773,#9813,#9814);
#8268=AXIS2_PLACEMENT_3D('',#12776,#9816,#9817);
#8269=AXIS2_PLACEMENT_3D('',#12777,#9818,#9819);
#8270=AXIS2_PLACEMENT_3D('',#12779,#9820,#9821);
#8271=AXIS2_PLACEMENT_3D('',#12782,#9823,#9824);
#8272=AXIS2_PLACEMENT_3D('',#12783,#9825,#9826);
#8273=AXIS2_PLACEMENT_3D('',#12785,#9827,#9828);
#8274=AXIS2_PLACEMENT_3D('',#12788,#9830,#9831);
#8275=AXIS2_PLACEMENT_3D('',#12789,#9832,#9833);
#8276=AXIS2_PLACEMENT_3D('',#12791,#9834,#9835);
#8277=AXIS2_PLACEMENT_3D('',#12794,#9837,#9838);
#8278=AXIS2_PLACEMENT_3D('',#12795,#9839,#9840);
#8279=AXIS2_PLACEMENT_3D('',#12796,#9841,#9842);
#8280=AXIS2_PLACEMENT_3D('',#12797,#9843,#9844);
#8281=AXIS2_PLACEMENT_3D('',#12798,#9845,#9846);
#8282=AXIS2_PLACEMENT_3D('',#12800,#9847,#9848);
#8283=AXIS2_PLACEMENT_3D('',#12803,#9850,#9851);
#8284=AXIS2_PLACEMENT_3D('',#12804,#9852,#9853);
#8285=AXIS2_PLACEMENT_3D('',#12806,#9854,#9855);
#8286=AXIS2_PLACEMENT_3D('',#12809,#9857,#9858);
#8287=AXIS2_PLACEMENT_3D('',#12810,#9859,#9860);
#8288=AXIS2_PLACEMENT_3D('',#12812,#9861,#9862);
#8289=AXIS2_PLACEMENT_3D('',#12815,#9864,#9865);
#8290=AXIS2_PLACEMENT_3D('',#12816,#9866,#9867);
#8291=AXIS2_PLACEMENT_3D('',#12818,#9868,#9869);
#8292=AXIS2_PLACEMENT_3D('',#12821,#9871,#9872);
#8293=AXIS2_PLACEMENT_3D('',#12822,#9873,#9874);
#8294=AXIS2_PLACEMENT_3D('',#12824,#9875,#9876);
#8295=AXIS2_PLACEMENT_3D('',#12827,#9878,#9879);
#8296=AXIS2_PLACEMENT_3D('',#12828,#9880,#9881);
#8297=AXIS2_PLACEMENT_3D('',#12830,#9882,#9883);
#8298=AXIS2_PLACEMENT_3D('',#12833,#9885,#9886);
#8299=AXIS2_PLACEMENT_3D('',#12834,#9887,#9888);
#8300=AXIS2_PLACEMENT_3D('',#12835,#9889,#9890);
#8301=AXIS2_PLACEMENT_3D('',#12836,#9891,#9892);
#8302=AXIS2_PLACEMENT_3D('',#12837,#9893,#9894);
#8303=AXIS2_PLACEMENT_3D('',#12839,#9895,#9896);
#8304=AXIS2_PLACEMENT_3D('',#12842,#9898,#9899);
#8305=AXIS2_PLACEMENT_3D('',#12843,#9900,#9901);
#8306=AXIS2_PLACEMENT_3D('',#12845,#9902,#9903);
#8307=AXIS2_PLACEMENT_3D('',#12848,#9905,#9906);
#8308=AXIS2_PLACEMENT_3D('',#12849,#9907,#9908);
#8309=AXIS2_PLACEMENT_3D('',#12850,#9909,#9910);
#8310=AXIS2_PLACEMENT_3D('',#12851,#9911,#9912);
#8311=AXIS2_PLACEMENT_3D('',#12852,#9913,#9914);
#8312=AXIS2_PLACEMENT_3D('',#12854,#9915,#9916);
#8313=AXIS2_PLACEMENT_3D('',#12857,#9918,#9919);
#8314=AXIS2_PLACEMENT_3D('',#12858,#9920,#9921);
#8315=AXIS2_PLACEMENT_3D('',#12860,#9922,#9923);
#8316=AXIS2_PLACEMENT_3D('',#12863,#9925,#9926);
#8317=AXIS2_PLACEMENT_3D('',#12864,#9927,#9928);
#8318=AXIS2_PLACEMENT_3D('',#12866,#9929,#9930);
#8319=AXIS2_PLACEMENT_3D('',#12869,#9932,#9933);
#8320=AXIS2_PLACEMENT_3D('',#12870,#9934,#9935);
#8321=AXIS2_PLACEMENT_3D('',#12872,#9936,#9937);
#8322=AXIS2_PLACEMENT_3D('',#12875,#9939,#9940);
#8323=AXIS2_PLACEMENT_3D('',#12876,#9941,#9942);
#8324=AXIS2_PLACEMENT_3D('',#12878,#9943,#9944);
#8325=AXIS2_PLACEMENT_3D('',#12881,#9946,#9947);
#8326=AXIS2_PLACEMENT_3D('',#12882,#9948,#9949);
#8327=AXIS2_PLACEMENT_3D('',#12884,#9950,#9951);
#8328=AXIS2_PLACEMENT_3D('',#12887,#9953,#9954);
#8329=AXIS2_PLACEMENT_3D('',#12888,#9955,#9956);
#8330=AXIS2_PLACEMENT_3D('',#12889,#9957,#9958);
#8331=AXIS2_PLACEMENT_3D('',#12890,#9959,#9960);
#8332=AXIS2_PLACEMENT_3D('',#12891,#9961,#9962);
#8333=AXIS2_PLACEMENT_3D('',#12893,#9963,#9964);
#8334=AXIS2_PLACEMENT_3D('',#12896,#9966,#9967);
#8335=AXIS2_PLACEMENT_3D('',#12897,#9968,#9969);
#8336=AXIS2_PLACEMENT_3D('',#12899,#9970,#9971);
#8337=AXIS2_PLACEMENT_3D('',#12902,#9973,#9974);
#8338=AXIS2_PLACEMENT_3D('',#12903,#9975,#9976);
#8339=AXIS2_PLACEMENT_3D('',#12905,#9977,#9978);
#8340=AXIS2_PLACEMENT_3D('',#12908,#9980,#9981);
#8341=AXIS2_PLACEMENT_3D('',#12909,#9982,#9983);
#8342=AXIS2_PLACEMENT_3D('',#12911,#9984,#9985);
#8343=AXIS2_PLACEMENT_3D('',#12914,#9987,#9988);
#8344=AXIS2_PLACEMENT_3D('',#12915,#9989,#9990);
#8345=AXIS2_PLACEMENT_3D('',#12917,#9991,#9992);
#8346=AXIS2_PLACEMENT_3D('',#12920,#9994,#9995);
#8347=AXIS2_PLACEMENT_3D('',#12921,#9996,#9997);
#8348=AXIS2_PLACEMENT_3D('',#12923,#9998,#9999);
#8349=AXIS2_PLACEMENT_3D('',#12926,#10001,#10002);
#8350=AXIS2_PLACEMENT_3D('',#12927,#10003,#10004);
#8351=AXIS2_PLACEMENT_3D('',#12928,#10005,#10006);
#8352=AXIS2_PLACEMENT_3D('',#12929,#10007,#10008);
#8353=AXIS2_PLACEMENT_3D('',#12930,#10009,#10010);
#8354=AXIS2_PLACEMENT_3D('',#12932,#10011,#10012);
#8355=AXIS2_PLACEMENT_3D('',#12935,#10014,#10015);
#8356=AXIS2_PLACEMENT_3D('',#12936,#10016,#10017);
#8357=AXIS2_PLACEMENT_3D('',#12945,#10022,#10023);
#8358=AXIS2_PLACEMENT_3D('',#12951,#10027,#10028);
#8359=AXIS2_PLACEMENT_3D('',#12957,#10032,#10033);
#8360=AXIS2_PLACEMENT_3D('',#12960,#10036,#10037);
#8361=AXIS2_PLACEMENT_3D('',#12961,#10038,#10039);
#8362=AXIS2_PLACEMENT_3D('',#12962,#10040,#10041);
#8363=AXIS2_PLACEMENT_3D('',#12963,#10042,#10043);
#8364=AXIS2_PLACEMENT_3D('',#12964,#10044,#10045);
#8365=AXIS2_PLACEMENT_3D('',#12966,#10046,#10047);
#8366=AXIS2_PLACEMENT_3D('',#12969,#10049,#10050);
#8367=AXIS2_PLACEMENT_3D('',#12970,#10051,#10052);
#8368=AXIS2_PLACEMENT_3D('',#12972,#10053,#10054);
#8369=AXIS2_PLACEMENT_3D('',#12975,#10056,#10057);
#8370=AXIS2_PLACEMENT_3D('',#12976,#10058,#10059);
#8371=AXIS2_PLACEMENT_3D('',#12978,#10060,#10061);
#8372=AXIS2_PLACEMENT_3D('',#12981,#10063,#10064);
#8373=AXIS2_PLACEMENT_3D('',#12982,#10065,#10066);
#8374=AXIS2_PLACEMENT_3D('',#12984,#10067,#10068);
#8375=AXIS2_PLACEMENT_3D('',#12987,#10070,#10071);
#8376=AXIS2_PLACEMENT_3D('',#12988,#10072,#10073);
#8377=AXIS2_PLACEMENT_3D('',#12990,#10074,#10075);
#8378=AXIS2_PLACEMENT_3D('',#12993,#10077,#10078);
#8379=AXIS2_PLACEMENT_3D('',#12994,#10079,#10080);
#8380=AXIS2_PLACEMENT_3D('',#12996,#10081,#10082);
#8381=AXIS2_PLACEMENT_3D('',#12999,#10084,#10085);
#8382=AXIS2_PLACEMENT_3D('',#13000,#10086,#10087);
#8383=AXIS2_PLACEMENT_3D('',#13002,#10088,#10089);
#8384=AXIS2_PLACEMENT_3D('',#13005,#10091,#10092);
#8385=AXIS2_PLACEMENT_3D('',#13006,#10093,#10094);
#8386=AXIS2_PLACEMENT_3D('',#13008,#10095,#10096);
#8387=AXIS2_PLACEMENT_3D('',#13011,#10098,#10099);
#8388=AXIS2_PLACEMENT_3D('',#13012,#10100,#10101);
#8389=AXIS2_PLACEMENT_3D('',#13014,#10102,#10103);
#8390=AXIS2_PLACEMENT_3D('',#13017,#10105,#10106);
#8391=AXIS2_PLACEMENT_3D('',#13018,#10107,#10108);
#8392=AXIS2_PLACEMENT_3D('',#13020,#10109,#10110);
#8393=AXIS2_PLACEMENT_3D('',#13023,#10112,#10113);
#8394=AXIS2_PLACEMENT_3D('',#13024,#10114,#10115);
#8395=AXIS2_PLACEMENT_3D('',#13029,#10117,#10118);
#8396=AXIS2_PLACEMENT_3D('',#13032,#10120,#10121);
#8397=AXIS2_PLACEMENT_3D('',#13033,#10122,#10123);
#8398=AXIS2_PLACEMENT_3D('',#13039,#10127,#10128);
#8399=AXIS2_PLACEMENT_3D('',#13042,#10130,#10131);
#8400=AXIS2_PLACEMENT_3D('',#13043,#10132,#10133);
#8401=AXIS2_PLACEMENT_3D('',#13047,#10136,#10137);
#8402=AXIS2_PLACEMENT_3D('',#13048,#10138,#10139);
#8403=AXIS2_PLACEMENT_3D('',#13049,#10140,#10141);
#8404=AXIS2_PLACEMENT_3D('',#13050,#10142,#10143);
#8405=AXIS2_PLACEMENT_3D('',#13051,#10144,#10145);
#8406=AXIS2_PLACEMENT_3D('',#13053,#10146,#10147);
#8407=AXIS2_PLACEMENT_3D('',#13056,#10149,#10150);
#8408=AXIS2_PLACEMENT_3D('',#13057,#10151,#10152);
#8409=AXIS2_PLACEMENT_3D('',#13059,#10153,#10154);
#8410=AXIS2_PLACEMENT_3D('',#13062,#10156,#10157);
#8411=AXIS2_PLACEMENT_3D('',#13063,#10158,#10159);
#8412=AXIS2_PLACEMENT_3D('',#13064,#10160,#10161);
#8413=AXIS2_PLACEMENT_3D('',#13065,#10162,#10163);
#8414=AXIS2_PLACEMENT_3D('',#13066,#10164,#10165);
#8415=AXIS2_PLACEMENT_3D('',#13068,#10166,#10167);
#8416=AXIS2_PLACEMENT_3D('',#13071,#10169,#10170);
#8417=AXIS2_PLACEMENT_3D('',#13072,#10171,#10172);
#8418=AXIS2_PLACEMENT_3D('',#13074,#10173,#10174);
#8419=AXIS2_PLACEMENT_3D('',#13077,#10176,#10177);
#8420=AXIS2_PLACEMENT_3D('',#13078,#10178,#10179);
#8421=AXIS2_PLACEMENT_3D('',#13080,#10180,#10181);
#8422=AXIS2_PLACEMENT_3D('',#13083,#10183,#10184);
#8423=AXIS2_PLACEMENT_3D('',#13084,#10185,#10186);
#8424=AXIS2_PLACEMENT_3D('',#13086,#10187,#10188);
#8425=AXIS2_PLACEMENT_3D('',#13089,#10190,#10191);
#8426=AXIS2_PLACEMENT_3D('',#13090,#10192,#10193);
#8427=AXIS2_PLACEMENT_3D('',#13092,#10194,#10195);
#8428=AXIS2_PLACEMENT_3D('',#13095,#10197,#10198);
#8429=AXIS2_PLACEMENT_3D('',#13096,#10199,#10200);
#8430=AXIS2_PLACEMENT_3D('',#13098,#10201,#10202);
#8431=AXIS2_PLACEMENT_3D('',#13101,#10204,#10205);
#8432=AXIS2_PLACEMENT_3D('',#13102,#10206,#10207);
#8433=AXIS2_PLACEMENT_3D('',#13103,#10208,#10209);
#8434=AXIS2_PLACEMENT_3D('',#13104,#10210,#10211);
#8435=AXIS2_PLACEMENT_3D('',#13105,#10212,#10213);
#8436=AXIS2_PLACEMENT_3D('',#13107,#10214,#10215);
#8437=AXIS2_PLACEMENT_3D('',#13110,#10217,#10218);
#8438=AXIS2_PLACEMENT_3D('',#13111,#10219,#10220);
#8439=AXIS2_PLACEMENT_3D('',#13113,#10221,#10222);
#8440=AXIS2_PLACEMENT_3D('',#13116,#10224,#10225);
#8441=AXIS2_PLACEMENT_3D('',#13117,#10226,#10227);
#8442=AXIS2_PLACEMENT_3D('',#13119,#10228,#10229);
#8443=AXIS2_PLACEMENT_3D('',#13122,#10231,#10232);
#8444=AXIS2_PLACEMENT_3D('',#13123,#10233,#10234);
#8445=AXIS2_PLACEMENT_3D('',#13125,#10235,#10236);
#8446=AXIS2_PLACEMENT_3D('',#13128,#10238,#10239);
#8447=AXIS2_PLACEMENT_3D('',#13129,#10240,#10241);
#8448=AXIS2_PLACEMENT_3D('',#13131,#10242,#10243);
#8449=AXIS2_PLACEMENT_3D('',#13134,#10245,#10246);
#8450=AXIS2_PLACEMENT_3D('',#13135,#10247,#10248);
#8451=AXIS2_PLACEMENT_3D('',#13137,#10249,#10250);
#8452=AXIS2_PLACEMENT_3D('',#13140,#10252,#10253);
#8453=AXIS2_PLACEMENT_3D('',#13141,#10254,#10255);
#8454=AXIS2_PLACEMENT_3D('',#13142,#10256,#10257);
#8455=AXIS2_PLACEMENT_3D('',#13143,#10258,#10259);
#8456=AXIS2_PLACEMENT_3D('',#13144,#10260,#10261);
#8457=AXIS2_PLACEMENT_3D('',#13146,#10262,#10263);
#8458=AXIS2_PLACEMENT_3D('',#13149,#10265,#10266);
#8459=AXIS2_PLACEMENT_3D('',#13150,#10267,#10268);
#8460=AXIS2_PLACEMENT_3D('',#13152,#10269,#10270);
#8461=AXIS2_PLACEMENT_3D('',#13155,#10272,#10273);
#8462=AXIS2_PLACEMENT_3D('',#13156,#10274,#10275);
#8463=AXIS2_PLACEMENT_3D('',#13157,#10276,#10277);
#8464=AXIS2_PLACEMENT_3D('',#13158,#10278,#10279);
#8465=AXIS2_PLACEMENT_3D('',#13159,#10280,#10281);
#8466=AXIS2_PLACEMENT_3D('',#13161,#10282,#10283);
#8467=AXIS2_PLACEMENT_3D('',#13164,#10285,#10286);
#8468=AXIS2_PLACEMENT_3D('',#13165,#10287,#10288);
#8469=AXIS2_PLACEMENT_3D('',#13167,#10289,#10290);
#8470=AXIS2_PLACEMENT_3D('',#13170,#10292,#10293);
#8471=AXIS2_PLACEMENT_3D('',#13171,#10294,#10295);
#8472=AXIS2_PLACEMENT_3D('',#13173,#10296,#10297);
#8473=AXIS2_PLACEMENT_3D('',#13176,#10299,#10300);
#8474=AXIS2_PLACEMENT_3D('',#13177,#10301,#10302);
#8475=AXIS2_PLACEMENT_3D('',#13179,#10303,#10304);
#8476=AXIS2_PLACEMENT_3D('',#13182,#10306,#10307);
#8477=AXIS2_PLACEMENT_3D('',#13183,#10308,#10309);
#8478=AXIS2_PLACEMENT_3D('',#13185,#10310,#10311);
#8479=AXIS2_PLACEMENT_3D('',#13188,#10313,#10314);
#8480=AXIS2_PLACEMENT_3D('',#13189,#10315,#10316);
#8481=AXIS2_PLACEMENT_3D('',#13191,#10317,#10318);
#8482=AXIS2_PLACEMENT_3D('',#13194,#10320,#10321);
#8483=AXIS2_PLACEMENT_3D('',#13195,#10322,#10323);
#8484=AXIS2_PLACEMENT_3D('',#13196,#10324,#10325);
#8485=AXIS2_PLACEMENT_3D('',#13197,#10326,#10327);
#8486=AXIS2_PLACEMENT_3D('',#13198,#10328,#10329);
#8487=AXIS2_PLACEMENT_3D('',#13200,#10330,#10331);
#8488=AXIS2_PLACEMENT_3D('',#13203,#10333,#10334);
#8489=AXIS2_PLACEMENT_3D('',#13204,#10335,#10336);
#8490=AXIS2_PLACEMENT_3D('',#13206,#10337,#10338);
#8491=AXIS2_PLACEMENT_3D('',#13209,#10340,#10341);
#8492=AXIS2_PLACEMENT_3D('',#13210,#10342,#10343);
#8493=AXIS2_PLACEMENT_3D('',#13212,#10344,#10345);
#8494=AXIS2_PLACEMENT_3D('',#13215,#10347,#10348);
#8495=AXIS2_PLACEMENT_3D('',#13216,#10349,#10350);
#8496=AXIS2_PLACEMENT_3D('',#13218,#10351,#10352);
#8497=AXIS2_PLACEMENT_3D('',#13221,#10354,#10355);
#8498=AXIS2_PLACEMENT_3D('',#13222,#10356,#10357);
#8499=AXIS2_PLACEMENT_3D('',#13224,#10358,#10359);
#8500=AXIS2_PLACEMENT_3D('',#13227,#10361,#10362);
#8501=AXIS2_PLACEMENT_3D('',#13228,#10363,#10364);
#8502=AXIS2_PLACEMENT_3D('',#13230,#10365,#10366);
#8503=AXIS2_PLACEMENT_3D('',#13233,#10368,#10369);
#8504=AXIS2_PLACEMENT_3D('',#13234,#10370,#10371);
#8505=AXIS2_PLACEMENT_3D('',#13235,#10372,#10373);
#8506=AXIS2_PLACEMENT_3D('',#13236,#10374,#10375);
#8507=AXIS2_PLACEMENT_3D('',#13237,#10376,#10377);
#8508=AXIS2_PLACEMENT_3D('',#13238,#10378,#10379);
#8509=AXIS2_PLACEMENT_3D('',#13241,#10380,#10381);
#8510=AXIS2_PLACEMENT_3D('',#13242,#10382,#10383);
#8511=AXIS2_PLACEMENT_3D('',#13244,#10384,#10385);
#8512=AXIS2_PLACEMENT_3D('',#13246,#10386,#10387);
#8513=AXIS2_PLACEMENT_3D('',#13247,#10388,#10389);
#8514=AXIS2_PLACEMENT_3D('',#13248,#10390,#10391);
#8515=AXIS2_PLACEMENT_3D('',#13251,#10393,#10394);
#8516=AXIS2_PLACEMENT_3D('',#13252,#10395,#10396);
#8517=AXIS2_PLACEMENT_3D('',#13254,#10397,#10398);
#8518=AXIS2_PLACEMENT_3D('',#13257,#10400,#10401);
#8519=AXIS2_PLACEMENT_3D('',#13258,#10402,#10403);
#8520=AXIS2_PLACEMENT_3D('',#13261,#10405,#10406);
#8521=AXIS2_PLACEMENT_3D('',#13262,#10407,#10408);
#8522=AXIS2_PLACEMENT_3D('',#13263,#10409,#10410);
#8523=AXIS2_PLACEMENT_3D('',#13265,#10411,#10412);
#8524=AXIS2_PLACEMENT_3D('',#13267,#10414,#10415);
#8525=AXIS2_PLACEMENT_3D('',#13269,#10416,#10417);
#8526=AXIS2_PLACEMENT_3D('',#13270,#10418,#10419);
#8527=AXIS2_PLACEMENT_3D('',#13272,#10421,#10422);
#8528=AXIS2_PLACEMENT_3D('',#13273,#10423,#10424);
#8529=AXIS2_PLACEMENT_3D('',#13276,#10425,#10426);
#8530=AXIS2_PLACEMENT_3D('',#13277,#10427,#10428);
#8531=AXIS2_PLACEMENT_3D('',#13279,#10429,#10430);
#8532=AXIS2_PLACEMENT_3D('',#13281,#10431,#10432);
#8533=AXIS2_PLACEMENT_3D('',#13282,#10433,#10434);
#8534=AXIS2_PLACEMENT_3D('',#13283,#10435,#10436);
#8535=AXIS2_PLACEMENT_3D('',#13285,#10437,#10438);
#8536=AXIS2_PLACEMENT_3D('',#13287,#10440,#10441);
#8537=AXIS2_PLACEMENT_3D('',#13289,#10442,#10443);
#8538=AXIS2_PLACEMENT_3D('',#13291,#10444,#10445);
#8539=AXIS2_PLACEMENT_3D('',#13292,#10446,#10447);
#8540=AXIS2_PLACEMENT_3D('',#13294,#10448,#10449);
#8541=AXIS2_PLACEMENT_3D('',#13296,#10451,#10452);
#8542=AXIS2_PLACEMENT_3D('',#13298,#10453,#10454);
#8543=AXIS2_PLACEMENT_3D('',#13300,#10456,#10457);
#8544=AXIS2_PLACEMENT_3D('',#13302,#10458,#10459);
#8545=AXIS2_PLACEMENT_3D('',#13304,#10461,#10462);
#8546=AXIS2_PLACEMENT_3D('',#13305,#10463,#10464);
#8547=AXIS2_PLACEMENT_3D('',#13307,#10466,#10467);
#8548=AXIS2_PLACEMENT_3D('',#13308,#10468,#10469);
#8549=AXIS2_PLACEMENT_3D('',#13311,#10470,#10471);
#8550=AXIS2_PLACEMENT_3D('',#13312,#10472,#10473);
#8551=AXIS2_PLACEMENT_3D('',#13315,#10474,#10475);
#8552=AXIS2_PLACEMENT_3D('',#13316,#10476,#10477);
#8553=AXIS2_PLACEMENT_3D('',#13319,#10478,#10479);
#8554=AXIS2_PLACEMENT_3D('',#13320,#10480,#10481);
#8555=AXIS2_PLACEMENT_3D('',#13323,#10482,#10483);
#8556=AXIS2_PLACEMENT_3D('',#13324,#10484,#10485);
#8557=AXIS2_PLACEMENT_3D('',#13327,#10486,#10487);
#8558=AXIS2_PLACEMENT_3D('',#13328,#10488,#10489);
#8559=AXIS2_PLACEMENT_3D('',#13331,#10490,#10491);
#8560=AXIS2_PLACEMENT_3D('',#13332,#10492,#10493);
#8561=AXIS2_PLACEMENT_3D('',#13335,#10494,#10495);
#8562=AXIS2_PLACEMENT_3D('',#13336,#10496,#10497);
#8563=AXIS2_PLACEMENT_3D('',#13339,#10498,#10499);
#8564=AXIS2_PLACEMENT_3D('',#13340,#10500,#10501);
#8565=AXIS2_PLACEMENT_3D('',#13341,#10502,#10503);
#8566=AXIS2_PLACEMENT_3D('',#13367,#10504,#10505);
#8567=AXIS2_PLACEMENT_3D('',#13391,#10506,#10507);
#8568=AXIS2_PLACEMENT_3D('',#13392,#10508,#10509);
#8569=AXIS2_PLACEMENT_3D('',#13394,#10510,#10511);
#8570=AXIS2_PLACEMENT_3D('',#13419,#10512,#10513);
#8571=AXIS2_PLACEMENT_3D('',#13444,#10514,#10515);
#8572=AXIS2_PLACEMENT_3D('',#13460,#10517,#10518);
#8573=AXIS2_PLACEMENT_3D('',#13475,#10519,#10520);
#8574=AXIS2_PLACEMENT_3D('',#13500,#10521,#10522);
#8575=AXIS2_PLACEMENT_3D('',#13525,#10523,#10524);
#8576=AXIS2_PLACEMENT_3D('',#13550,#10525,#10526);
#8577=AXIS2_PLACEMENT_3D('',#13574,#10527,#10528);
#8578=AXIS2_PLACEMENT_3D('',#13575,#10529,#10530);
#8579=AXIS2_PLACEMENT_3D('',#13577,#10531,#10532);
#8580=AXIS2_PLACEMENT_3D('',#13578,#10533,#10534);
#8581=AXIS2_PLACEMENT_3D('',#13579,#10535,#10536);
#8582=AXIS2_PLACEMENT_3D('',#13603,#10537,#10538);
#8583=AXIS2_PLACEMENT_3D('',#13604,#10539,#10540);
#8584=AXIS2_PLACEMENT_3D('',#13606,#10541,#10542);
#8585=AXIS2_PLACEMENT_3D('',#13607,#10543,#10544);
#8586=AXIS2_PLACEMENT_3D('',#13608,#10545,#10546);
#8587=AXIS2_PLACEMENT_3D('',#13632,#10547,#10548);
#8588=AXIS2_PLACEMENT_3D('',#13633,#10549,#10550);
#8589=AXIS2_PLACEMENT_3D('',#13635,#10551,#10552);
#8590=AXIS2_PLACEMENT_3D('',#13636,#10553,#10554);
#8591=AXIS2_PLACEMENT_3D('',#13637,#10555,#10556);
#8592=AXIS2_PLACEMENT_3D('',#13652,#10557,#10558);
#8593=AXIS2_PLACEMENT_3D('',#13665,#10559,#10560);
#8594=AXIS2_PLACEMENT_3D('',#13667,#10561,#10562);
#8595=AXIS2_PLACEMENT_3D('',#13668,#10563,#10564);
#8596=AXIS2_PLACEMENT_3D('',#13669,#10565,#10566);
#8597=AXIS2_PLACEMENT_3D('',#13693,#10567,#10568);
#8598=AXIS2_PLACEMENT_3D('',#13694,#10569,#10570);
#8599=AXIS2_PLACEMENT_3D('',#13696,#10571,#10572);
#8600=AXIS2_PLACEMENT_3D('',#13697,#10573,#10574);
#8601=AXIS2_PLACEMENT_3D('',#13698,#10575,#10576);
#8602=AXIS2_PLACEMENT_3D('',#13722,#10577,#10578);
#8603=AXIS2_PLACEMENT_3D('',#13723,#10579,#10580);
#8604=AXIS2_PLACEMENT_3D('',#13725,#10581,#10582);
#8605=AXIS2_PLACEMENT_3D('',#13726,#10583,#10584);
#8606=AXIS2_PLACEMENT_3D('',#13727,#10585,#10586);
#8607=AXIS2_PLACEMENT_3D('',#13751,#10587,#10588);
#8608=AXIS2_PLACEMENT_3D('',#13752,#10589,#10590);
#8609=AXIS2_PLACEMENT_3D('',#13754,#10591,#10592);
#8610=AXIS2_PLACEMENT_3D('',#13757,#10594,#10595);
#8611=AXIS2_PLACEMENT_3D('',#13781,#10596,#10597);
#8612=AXIS2_PLACEMENT_3D('',#13782,#10598,#10599);
#8613=AXIS2_PLACEMENT_3D('',#13783,#10600,#10601);
#8614=AXIS2_PLACEMENT_3D('',#13784,#10602,#10603);
#8615=AXIS2_PLACEMENT_3D('',#13785,#10604,#10605);
#8616=AXIS2_PLACEMENT_3D('',#13786,#10606,#10607);
#8617=AXIS2_PLACEMENT_3D('',#13787,#10608,#10609);
#8618=AXIS2_PLACEMENT_3D('',#13788,#10610,#10611);
#8619=AXIS2_PLACEMENT_3D('',#13789,#10612,#10613);
#8620=AXIS2_PLACEMENT_3D('',#13791,#10614,#10615);
#8621=AXIS2_PLACEMENT_3D('',#13793,#10616,#10617);
#8622=AXIS2_PLACEMENT_3D('',#13794,#10618,#10619);
#8623=AXIS2_PLACEMENT_3D('',#13796,#10620,#10621);
#8624=AXIS2_PLACEMENT_3D('',#13798,#10623,#10624);
#8625=AXIS2_PLACEMENT_3D('',#13800,#10625,#10626);
#8626=AXIS2_PLACEMENT_3D('',#13801,#10627,#10628);
#8627=AXIS2_PLACEMENT_3D('',#13803,#10630,#10631);
#8628=AXIS2_PLACEMENT_3D('',#13805,#10632,#10633);
#8629=AXIS2_PLACEMENT_3D('',#13807,#10634,#10635);
#8630=AXIS2_PLACEMENT_3D('',#13808,#10636,#10637);
#8631=AXIS2_PLACEMENT_3D('',#13810,#10638,#10639);
#8632=AXIS2_PLACEMENT_3D('',#13812,#10641,#10642);
#8633=AXIS2_PLACEMENT_3D('',#13814,#10643,#10644);
#8634=AXIS2_PLACEMENT_3D('',#13815,#10645,#10646);
#8635=AXIS2_PLACEMENT_3D('',#13817,#10648,#10649);
#8636=AXIS2_PLACEMENT_3D('',#13818,#10650,#10651);
#8637=AXIS2_PLACEMENT_3D('',#13819,#10652,#10653);
#8638=AXIS2_PLACEMENT_3D('',#13820,#10654,#10655);
#8639=AXIS2_PLACEMENT_3D('',#13821,#10656,#10657);
#8640=AXIS2_PLACEMENT_3D('',#13822,#10658,#10659);
#8641=AXIS2_PLACEMENT_3D('',#13823,#10660,#10661);
#8642=AXIS2_PLACEMENT_3D('',#13832,#10666,#10667);
#8643=AXIS2_PLACEMENT_3D('',#13838,#10671,#10672);
#8644=AXIS2_PLACEMENT_3D('',#13844,#10676,#10677);
#8645=AXIS2_PLACEMENT_3D('',#13850,#10681,#10682);
#8646=AXIS2_PLACEMENT_3D('',#13856,#10686,#10687);
#8647=AXIS2_PLACEMENT_3D('',#13859,#10690,#10691);
#8648=AXIS2_PLACEMENT_3D('',#13860,#10692,#10693);
#8649=AXIS2_PLACEMENT_3D('',#13861,#10694,#10695);
#8650=AXIS2_PLACEMENT_3D('',#13863,#10696,#10697);
#8651=AXIS2_PLACEMENT_3D('',#13864,#10698,#10699);
#8652=AXIS2_PLACEMENT_3D('',#13866,#10700,#10701);
#8653=AXIS2_PLACEMENT_3D('',#13867,#10702,#10703);
#8654=AXIS2_PLACEMENT_3D('',#13869,#10704,#10705);
#8655=AXIS2_PLACEMENT_3D('',#13871,#10707,#10708);
#8656=AXIS2_PLACEMENT_3D('',#13873,#10709,#10710);
#8657=AXIS2_PLACEMENT_3D('',#13875,#10712,#10713);
#8658=AXIS2_PLACEMENT_3D('',#13877,#10714,#10715);
#8659=AXIS2_PLACEMENT_3D('',#13879,#10717,#10718);
#8660=AXIS2_PLACEMENT_3D('',#13881,#10719,#10720);
#8661=AXIS2_PLACEMENT_3D('',#13882,#10721,#10722);
#8662=AXIS2_PLACEMENT_3D('',#13884,#10723,#10724);
#8663=AXIS2_PLACEMENT_3D('',#13886,#10726,#10727);
#8664=AXIS2_PLACEMENT_3D('',#13888,#10729,#10730);
#8665=AXIS2_PLACEMENT_3D('',#13889,#10731,#10732);
#8666=AXIS2_PLACEMENT_3D('',#13890,#10733,#10734);
#8667=AXIS2_PLACEMENT_3D('',#13891,#10735,#10736);
#8668=AXIS2_PLACEMENT_3D('',#13892,#10737,#10738);
#8669=AXIS2_PLACEMENT_3D('',#13893,#10739,#10740);
#8670=AXIS2_PLACEMENT_3D('',#13894,#10741,#10742);
#8671=AXIS2_PLACEMENT_3D('',#13895,#10743,#10744);
#8672=AXIS2_PLACEMENT_3D('',#13896,#10745,#10746);
#8673=AXIS2_PLACEMENT_3D('',#13897,#10747,#10748);
#8674=AXIS2_PLACEMENT_3D('',#13898,#10749,#10750);
#8675=AXIS2_PLACEMENT_3D('',#13899,#10751,#10752);
#8676=AXIS2_PLACEMENT_3D('',#13900,#10753,#10754);
#8677=AXIS2_PLACEMENT_3D('',#13901,#10755,#10756);
#8678=AXIS2_PLACEMENT_3D('',#13902,#10757,#10758);
#8679=AXIS2_PLACEMENT_3D('',#13903,#10759,#10760);
#8680=AXIS2_PLACEMENT_3D('',#13904,#10761,#10762);
#8681=AXIS2_PLACEMENT_3D('',#13905,#10763,#10764);
#8682=AXIS2_PLACEMENT_3D('',#13906,#10765,#10766);
#8683=AXIS2_PLACEMENT_3D('',#13907,#10767,#10768);
#8684=AXIS2_PLACEMENT_3D('',#13908,#10769,#10770);
#8685=AXIS2_PLACEMENT_3D('',#13909,#10771,#10772);
#8686=AXIS2_PLACEMENT_3D('',#13910,#10773,#10774);
#8687=AXIS2_PLACEMENT_3D('',#13911,#10775,#10776);
#8688=AXIS2_PLACEMENT_3D('',#13912,#10777,#10778);
#8689=AXIS2_PLACEMENT_3D('',#13913,#10779,#10780);
#8690=AXIS2_PLACEMENT_3D('',#13914,#10781,#10782);
#8691=AXIS2_PLACEMENT_3D('',#13915,#10783,#10784);
#8692=AXIS2_PLACEMENT_3D('',#13916,#10785,#10786);
#8693=AXIS2_PLACEMENT_3D('',#13917,#10787,#10788);
#8694=AXIS2_PLACEMENT_3D('',#13918,#10789,#10790);
#8695=AXIS2_PLACEMENT_3D('',#13919,#10791,#10792);
#8696=AXIS2_PLACEMENT_3D('',#13920,#10793,#10794);
#8697=AXIS2_PLACEMENT_3D('',#13921,#10795,#10796);
#8698=AXIS2_PLACEMENT_3D('',#13922,#10797,#10798);
#8699=AXIS2_PLACEMENT_3D('',#13923,#10799,#10800);
#8700=AXIS2_PLACEMENT_3D('',#13924,#10801,#10802);
#8701=AXIS2_PLACEMENT_3D('',#13925,#10803,#10804);
#8702=AXIS2_PLACEMENT_3D('',#13926,#10805,#10806);
#8703=AXIS2_PLACEMENT_3D('',#13927,#10807,#10808);
#8704=AXIS2_PLACEMENT_3D('',#13928,#10809,#10810);
#8705=AXIS2_PLACEMENT_3D('',#13929,#10811,#10812);
#8706=AXIS2_PLACEMENT_3D('',#13930,#10813,#10814);
#8707=AXIS2_PLACEMENT_3D('',#13931,#10815,#10816);
#8708=AXIS2_PLACEMENT_3D('',#13932,#10817,#10818);
#8709=AXIS2_PLACEMENT_3D('',#13933,#10819,#10820);
#8710=AXIS2_PLACEMENT_3D('',#13934,#10821,#10822);
#8711=AXIS2_PLACEMENT_3D('',#13935,#10823,#10824);
#8712=AXIS2_PLACEMENT_3D('',#13936,#10825,#10826);
#8713=AXIS2_PLACEMENT_3D('',#13937,#10827,#10828);
#8714=AXIS2_PLACEMENT_3D('',#13938,#10829,#10830);
#8715=AXIS2_PLACEMENT_3D('',#13939,#10831,#10832);
#8716=AXIS2_PLACEMENT_3D('',#13940,#10833,#10834);
#8717=AXIS2_PLACEMENT_3D('',#13941,#10835,#10836);
#8718=AXIS2_PLACEMENT_3D('',#13942,#10837,#10838);
#8719=AXIS2_PLACEMENT_3D('',#13943,#10839,#10840);
#8720=AXIS2_PLACEMENT_3D('',#13944,#10841,#10842);
#8721=AXIS2_PLACEMENT_3D('',#13945,#10843,#10844);
#8722=AXIS2_PLACEMENT_3D('',#13947,#10845,#10846);
#8723=AXIS2_PLACEMENT_3D('',#13950,#10848,#10849);
#8724=AXIS2_PLACEMENT_3D('',#13951,#10850,#10851);
#8725=AXIS2_PLACEMENT_3D('',#13953,#10852,#10853);
#8726=AXIS2_PLACEMENT_3D('',#13956,#10855,#10856);
#8727=AXIS2_PLACEMENT_3D('',#13957,#10857,#10858);
#8728=AXIS2_PLACEMENT_3D('',#13959,#10859,#10860);
#8729=AXIS2_PLACEMENT_3D('',#13962,#10862,#10863);
#8730=AXIS2_PLACEMENT_3D('',#13963,#10864,#10865);
#8731=AXIS2_PLACEMENT_3D('',#13965,#10866,#10867);
#8732=AXIS2_PLACEMENT_3D('',#13968,#10869,#10870);
#8733=AXIS2_PLACEMENT_3D('',#13969,#10871,#10872);
#8734=AXIS2_PLACEMENT_3D('',#13971,#10873,#10874);
#8735=AXIS2_PLACEMENT_3D('',#13974,#10876,#10877);
#8736=AXIS2_PLACEMENT_3D('',#13975,#10878,#10879);
#8737=AXIS2_PLACEMENT_3D('',#13977,#10880,#10881);
#8738=AXIS2_PLACEMENT_3D('',#13980,#10883,#10884);
#8739=AXIS2_PLACEMENT_3D('',#13981,#10885,#10886);
#8740=AXIS2_PLACEMENT_3D('',#13983,#10887,#10888);
#8741=AXIS2_PLACEMENT_3D('',#13986,#10890,#10891);
#8742=AXIS2_PLACEMENT_3D('',#13987,#10892,#10893);
#8743=AXIS2_PLACEMENT_3D('',#13989,#10894,#10895);
#8744=AXIS2_PLACEMENT_3D('',#13992,#10897,#10898);
#8745=AXIS2_PLACEMENT_3D('',#13993,#10899,#10900);
#8746=AXIS2_PLACEMENT_3D('',#13995,#10901,#10902);
#8747=AXIS2_PLACEMENT_3D('',#13998,#10904,#10905);
#8748=AXIS2_PLACEMENT_3D('',#13999,#10906,#10907);
#8749=AXIS2_PLACEMENT_3D('',#14001,#10908,#10909);
#8750=AXIS2_PLACEMENT_3D('',#14004,#10911,#10912);
#8751=AXIS2_PLACEMENT_3D('',#14005,#10913,#10914);
#8752=AXIS2_PLACEMENT_3D('',#14007,#10915,#10916);
#8753=AXIS2_PLACEMENT_3D('',#14010,#10918,#10919);
#8754=AXIS2_PLACEMENT_3D('',#14011,#10920,#10921);
#8755=AXIS2_PLACEMENT_3D('',#14013,#10922,#10923);
#8756=AXIS2_PLACEMENT_3D('',#14016,#10925,#10926);
#8757=AXIS2_PLACEMENT_3D('',#14017,#10927,#10928);
#8758=AXIS2_PLACEMENT_3D('',#14026,#10933,#10934);
#8759=AXIS2_PLACEMENT_3D('',#14032,#10938,#10939);
#8760=AXIS2_PLACEMENT_3D('',#14036,#10942,#10943);
#8761=AXIS2_PLACEMENT_3D('',#14044,#10948,#10949);
#8762=AXIS2_PLACEMENT_3D('',#14050,#10953,#10954);
#8763=AXIS2_PLACEMENT_3D('',#14054,#10957,#10958);
#8764=AXIS2_PLACEMENT_3D('',#14058,#10961,#10962);
#8765=AXIS2_PLACEMENT_3D('',#14060,#10964,#10965);
#8766=AXIS2_PLACEMENT_3D('',#14061,#10966,#10967);
#8767=AXIS2_PLACEMENT_3D('',#14062,#10968,#10969);
#8768=AXIS2_PLACEMENT_3D('',#14064,#10970,#10971);
#8769=AXIS2_PLACEMENT_3D('',#14067,#10973,#10974);
#8770=AXIS2_PLACEMENT_3D('',#14068,#10975,#10976);
#8771=AXIS2_PLACEMENT_3D('',#14069,#10977,#10978);
#8772=AXIS2_PLACEMENT_3D('',#14071,#10979,#10980);
#8773=AXIS2_PLACEMENT_3D('',#14074,#10982,#10983);
#8774=AXIS2_PLACEMENT_3D('',#14075,#10984,#10985);
#8775=AXIS2_PLACEMENT_3D('',#14077,#10986,#10987);
#8776=AXIS2_PLACEMENT_3D('',#14080,#10989,#10990);
#8777=AXIS2_PLACEMENT_3D('',#14081,#10991,#10992);
#8778=AXIS2_PLACEMENT_3D('',#14083,#10993,#10994);
#8779=AXIS2_PLACEMENT_3D('',#14086,#10996,#10997);
#8780=AXIS2_PLACEMENT_3D('',#14087,#10998,#10999);
#8781=AXIS2_PLACEMENT_3D('',#14089,#11000,#11001);
#8782=AXIS2_PLACEMENT_3D('',#14091,#11002,#11003);
#8783=AXIS2_PLACEMENT_3D('',#14092,#11004,#11005);
#8784=AXIS2_PLACEMENT_3D('',#14094,#11006,#11007);
#8785=AXIS2_PLACEMENT_3D('',#14096,#11008,#11009);
#8786=AXIS2_PLACEMENT_3D('',#14097,#11010,#11011);
#8787=AXIS2_PLACEMENT_3D('',#14099,#11013,#11014);
#8788=AXIS2_PLACEMENT_3D('',#14102,#11016,#11017);
#8789=AXIS2_PLACEMENT_3D('',#14103,#11018,#11019);
#8790=AXIS2_PLACEMENT_3D('',#14105,#11020,#11021);
#8791=AXIS2_PLACEMENT_3D('',#14107,#11023,#11024);
#8792=AXIS2_PLACEMENT_3D('',#14108,#11025,#11026);
#8793=AXIS2_PLACEMENT_3D('',#14109,#11027,#11028);
#8794=AXIS2_PLACEMENT_3D('',#14110,#11029,#11030);
#8795=AXIS2_PLACEMENT_3D('',#14112,#11031,#11032);
#8796=AXIS2_PLACEMENT_3D('',#14115,#11034,#11035);
#8797=AXIS2_PLACEMENT_3D('',#14116,#11036,#11037);
#8798=AXIS2_PLACEMENT_3D('',#14118,#11038,#11039);
#8799=AXIS2_PLACEMENT_3D('',#14121,#11041,#11042);
#8800=AXIS2_PLACEMENT_3D('',#14122,#11043,#11044);
#8801=AXIS2_PLACEMENT_3D('',#14123,#11045,#11046);
#8802=AXIS2_PLACEMENT_3D('',#14124,#11047,#11048);
#8803=AXIS2_PLACEMENT_3D('',#14125,#11049,#11050);
#8804=AXIS2_PLACEMENT_3D('',#14127,#11051,#11052);
#8805=AXIS2_PLACEMENT_3D('',#14130,#11054,#11055);
#8806=AXIS2_PLACEMENT_3D('',#14131,#11056,#11057);
#8807=AXIS2_PLACEMENT_3D('',#14133,#11058,#11059);
#8808=AXIS2_PLACEMENT_3D('',#14136,#11061,#11062);
#8809=AXIS2_PLACEMENT_3D('',#14137,#11063,#11064);
#8810=AXIS2_PLACEMENT_3D('',#14138,#11065,#11066);
#8811=AXIS2_PLACEMENT_3D('',#14139,#11067,#11068);
#8812=AXIS2_PLACEMENT_3D('',#14140,#11069,#11070);
#8813=AXIS2_PLACEMENT_3D('',#14142,#11071,#11072);
#8814=AXIS2_PLACEMENT_3D('',#14145,#11074,#11075);
#8815=AXIS2_PLACEMENT_3D('',#14146,#11076,#11077);
#8816=AXIS2_PLACEMENT_3D('',#14148,#11078,#11079);
#8817=AXIS2_PLACEMENT_3D('',#14151,#11081,#11082);
#8818=AXIS2_PLACEMENT_3D('',#14152,#11083,#11084);
#8819=AXIS2_PLACEMENT_3D('',#14153,#11085,#11086);
#8820=AXIS2_PLACEMENT_3D('',#14154,#11087,#11088);
#8821=AXIS2_PLACEMENT_3D('',#14155,#11089,#11090);
#8822=AXIS2_PLACEMENT_3D('',#14157,#11091,#11092);
#8823=AXIS2_PLACEMENT_3D('',#14160,#11094,#11095);
#8824=AXIS2_PLACEMENT_3D('',#14161,#11096,#11097);
#8825=AXIS2_PLACEMENT_3D('',#14163,#11098,#11099);
#8826=AXIS2_PLACEMENT_3D('',#14166,#11101,#11102);
#8827=AXIS2_PLACEMENT_3D('',#14167,#11103,#11104);
#8828=AXIS2_PLACEMENT_3D('',#14168,#11105,#11106);
#8829=AXIS2_PLACEMENT_3D('',#14169,#11107,#11108);
#8830=AXIS2_PLACEMENT_3D('',#14170,#11109,#11110);
#8831=AXIS2_PLACEMENT_3D('',#14172,#11111,#11112);
#8832=AXIS2_PLACEMENT_3D('',#14175,#11114,#11115);
#8833=AXIS2_PLACEMENT_3D('',#14176,#11116,#11117);
#8834=AXIS2_PLACEMENT_3D('',#14177,#11118,#11119);
#8835=AXIS2_PLACEMENT_3D('',#14179,#11120,#11121);
#8836=AXIS2_PLACEMENT_3D('',#14182,#11123,#11124);
#8837=AXIS2_PLACEMENT_3D('',#14183,#11125,#11126);
#8838=AXIS2_PLACEMENT_3D('',#14185,#11127,#11128);
#8839=AXIS2_PLACEMENT_3D('',#14188,#11130,#11131);
#8840=AXIS2_PLACEMENT_3D('',#14189,#11132,#11133);
#8841=AXIS2_PLACEMENT_3D('',#14191,#11134,#11135);
#8842=AXIS2_PLACEMENT_3D('',#14194,#11137,#11138);
#8843=AXIS2_PLACEMENT_3D('',#14195,#11139,#11140);
#8844=AXIS2_PLACEMENT_3D('',#14197,#11141,#11142);
#8845=AXIS2_PLACEMENT_3D('',#14199,#11143,#11144);
#8846=AXIS2_PLACEMENT_3D('',#14200,#11145,#11146);
#8847=AXIS2_PLACEMENT_3D('',#14202,#11147,#11148);
#8848=AXIS2_PLACEMENT_3D('',#14204,#11149,#11150);
#8849=AXIS2_PLACEMENT_3D('',#14205,#11151,#11152);
#8850=AXIS2_PLACEMENT_3D('',#14207,#11154,#11155);
#8851=AXIS2_PLACEMENT_3D('',#14210,#11157,#11158);
#8852=AXIS2_PLACEMENT_3D('',#14211,#11159,#11160);
#8853=AXIS2_PLACEMENT_3D('',#14213,#11161,#11162);
#8854=AXIS2_PLACEMENT_3D('',#14215,#11164,#11165);
#8855=AXIS2_PLACEMENT_3D('',#14216,#11166,#11167);
#8856=AXIS2_PLACEMENT_3D('',#14217,#11168,#11169);
#8857=AXIS2_PLACEMENT_3D('',#14218,#11170,#11171);
#8858=AXIS2_PLACEMENT_3D('',#14220,#11172,#11173);
#8859=AXIS2_PLACEMENT_3D('',#14223,#11175,#11176);
#8860=AXIS2_PLACEMENT_3D('',#14224,#11177,#11178);
#8861=AXIS2_PLACEMENT_3D('',#14226,#11179,#11180);
#8862=AXIS2_PLACEMENT_3D('',#14229,#11182,#11183);
#8863=AXIS2_PLACEMENT_3D('',#14230,#11184,#11185);
#8864=AXIS2_PLACEMENT_3D('',#14231,#11186,#11187);
#8865=AXIS2_PLACEMENT_3D('',#14232,#11188,#11189);
#8866=AXIS2_PLACEMENT_3D('',#14233,#11190,#11191);
#8867=AXIS2_PLACEMENT_3D('',#14235,#11192,#11193);
#8868=AXIS2_PLACEMENT_3D('',#14238,#11195,#11196);
#8869=AXIS2_PLACEMENT_3D('',#14239,#11197,#11198);
#8870=AXIS2_PLACEMENT_3D('',#14241,#11199,#11200);
#8871=AXIS2_PLACEMENT_3D('',#14244,#11202,#11203);
#8872=AXIS2_PLACEMENT_3D('',#14245,#11204,#11205);
#8873=AXIS2_PLACEMENT_3D('',#14246,#11206,#11207);
#8874=AXIS2_PLACEMENT_3D('',#14247,#11208,#11209);
#8875=AXIS2_PLACEMENT_3D('',#14248,#11210,#11211);
#8876=AXIS2_PLACEMENT_3D('',#14250,#11212,#11213);
#8877=AXIS2_PLACEMENT_3D('',#14253,#11215,#11216);
#8878=AXIS2_PLACEMENT_3D('',#14254,#11217,#11218);
#8879=AXIS2_PLACEMENT_3D('',#14256,#11219,#11220);
#8880=AXIS2_PLACEMENT_3D('',#14259,#11222,#11223);
#8881=AXIS2_PLACEMENT_3D('',#14260,#11224,#11225);
#8882=AXIS2_PLACEMENT_3D('',#14261,#11226,#11227);
#8883=AXIS2_PLACEMENT_3D('',#14262,#11228,#11229);
#8884=AXIS2_PLACEMENT_3D('',#14263,#11230,#11231);
#8885=AXIS2_PLACEMENT_3D('',#14265,#11232,#11233);
#8886=AXIS2_PLACEMENT_3D('',#14268,#11235,#11236);
#8887=AXIS2_PLACEMENT_3D('',#14269,#11237,#11238);
#8888=AXIS2_PLACEMENT_3D('',#14271,#11239,#11240);
#8889=AXIS2_PLACEMENT_3D('',#14274,#11242,#11243);
#8890=AXIS2_PLACEMENT_3D('',#14275,#11244,#11245);
#8891=AXIS2_PLACEMENT_3D('',#14276,#11246,#11247);
#8892=AXIS2_PLACEMENT_3D('',#14277,#11248,#11249);
#8893=AXIS2_PLACEMENT_3D('',#14278,#11250,#11251);
#8894=AXIS2_PLACEMENT_3D('',#14280,#11252,#11253);
#8895=AXIS2_PLACEMENT_3D('',#14281,#11254,#11255);
#8896=AXIS2_PLACEMENT_3D('',#14283,#11256,#11257);
#8897=AXIS2_PLACEMENT_3D('',#14285,#11259,#11260);
#8898=AXIS2_PLACEMENT_3D('',#14287,#11261,#11262);
#8899=AXIS2_PLACEMENT_3D('',#14289,#11264,#11265);
#8900=AXIS2_PLACEMENT_3D('',#14291,#11266,#11267);
#8901=AXIS2_PLACEMENT_3D('',#14293,#11269,#11270);
#8902=AXIS2_PLACEMENT_3D('',#14295,#11271,#11272);
#8903=AXIS2_PLACEMENT_3D('',#14296,#11273,#11274);
#8904=AXIS2_PLACEMENT_3D('',#14298,#11275,#11276);
#8905=AXIS2_PLACEMENT_3D('',#14300,#11278,#11279);
#8906=AXIS2_PLACEMENT_3D('',#14302,#11280,#11281);
#8907=AXIS2_PLACEMENT_3D('',#14304,#11283,#11284);
#8908=AXIS2_PLACEMENT_3D('',#14306,#11285,#11286);
#8909=AXIS2_PLACEMENT_3D('',#14308,#11288,#11289);
#8910=AXIS2_PLACEMENT_3D('',#14309,#11290,#11291);
#8911=AXIS2_PLACEMENT_3D('',#14318,#11296,#11297);
#8912=AXIS2_PLACEMENT_3D('',#14324,#11301,#11302);
#8913=AXIS2_PLACEMENT_3D('',#14330,#11306,#11307);
#8914=AXIS2_PLACEMENT_3D('',#14336,#11311,#11312);
#8915=AXIS2_PLACEMENT_3D('',#14342,#11316,#11317);
#8916=AXIS2_PLACEMENT_3D('',#14345,#11320,#11321);
#8917=AXIS2_PLACEMENT_3D('',#14346,#11322,#11323);
#8918=AXIS2_PLACEMENT_3D('',#14347,#11324,#11325);
#8919=AXIS2_PLACEMENT_3D('',#14348,#11326,#11327);
#8920=AXIS2_PLACEMENT_3D('',#14349,#11328,#11329);
#8921=AXIS2_PLACEMENT_3D('',#14350,#11330,#11331);
#8922=AXIS2_PLACEMENT_3D('',#14351,#11332,#11333);
#8923=AXIS2_PLACEMENT_3D('',#14352,#11334,#11335);
#8924=AXIS2_PLACEMENT_3D('',#14353,#11336,#11337);
#8925=AXIS2_PLACEMENT_3D('',#14354,#11338,#11339);
#8926=AXIS2_PLACEMENT_3D('',#14355,#11340,#11341);
#8927=AXIS2_PLACEMENT_3D('',#14356,#11342,#11343);
#8928=AXIS2_PLACEMENT_3D('',#14357,#11344,#11345);
#8929=AXIS2_PLACEMENT_3D('',#14358,#11346,#11347);
#8930=AXIS2_PLACEMENT_3D('',#14359,#11348,#11349);
#8931=AXIS2_PLACEMENT_3D('',#14360,#11350,#11351);
#8932=AXIS2_PLACEMENT_3D('',#14361,#11352,#11353);
#8933=AXIS2_PLACEMENT_3D('',#14362,#11354,#11355);
#8934=AXIS2_PLACEMENT_3D('',#14363,#11356,#11357);
#8935=AXIS2_PLACEMENT_3D('',#14364,#11358,#11359);
#8936=AXIS2_PLACEMENT_3D('',#14365,#11360,#11361);
#8937=AXIS2_PLACEMENT_3D('',#14366,#11362,#11363);
#8938=AXIS2_PLACEMENT_3D('',#14367,#11364,#11365);
#8939=AXIS2_PLACEMENT_3D('',#14368,#11366,#11367);
#8940=AXIS2_PLACEMENT_3D('',#14369,#11368,#11369);
#8941=AXIS2_PLACEMENT_3D('',#14370,#11370,#11371);
#8942=AXIS2_PLACEMENT_3D('',#14371,#11372,#11373);
#8943=AXIS2_PLACEMENT_3D('',#14372,#11374,#11375);
#8944=AXIS2_PLACEMENT_3D('',#14373,#11376,#11377);
#8945=AXIS2_PLACEMENT_3D('',#14374,#11378,#11379);
#8946=AXIS2_PLACEMENT_3D('',#14375,#11380,#11381);
#8947=AXIS2_PLACEMENT_3D('',#14376,#11382,#11383);
#8948=AXIS2_PLACEMENT_3D('',#14377,#11384,#11385);
#8949=AXIS2_PLACEMENT_3D('',#14378,#11386,#11387);
#8950=AXIS2_PLACEMENT_3D('',#14379,#11388,#11389);
#8951=AXIS2_PLACEMENT_3D('',#14380,#11390,#11391);
#8952=AXIS2_PLACEMENT_3D('',#14381,#11392,#11393);
#8953=AXIS2_PLACEMENT_3D('',#14382,#11394,#11395);
#8954=AXIS2_PLACEMENT_3D('',#14383,#11396,#11397);
#8955=AXIS2_PLACEMENT_3D('',#14384,#11398,#11399);
#8956=AXIS2_PLACEMENT_3D('',#14385,#11400,#11401);
#8957=AXIS2_PLACEMENT_3D('',#14386,#11402,#11403);
#8958=AXIS2_PLACEMENT_3D('',#14387,#11404,#11405);
#8959=AXIS2_PLACEMENT_3D('',#14388,#11406,#11407);
#8960=AXIS2_PLACEMENT_3D('',#14389,#11408,#11409);
#8961=AXIS2_PLACEMENT_3D('',#14390,#11410,#11411);
#8962=AXIS2_PLACEMENT_3D('',#14391,#11412,#11413);
#8963=AXIS2_PLACEMENT_3D('',#14392,#11414,#11415);
#8964=AXIS2_PLACEMENT_3D('',#14393,#11416,#11417);
#8965=AXIS2_PLACEMENT_3D('',#14394,#11418,#11419);
#8966=AXIS2_PLACEMENT_3D('',#14395,#11420,#11421);
#8967=AXIS2_PLACEMENT_3D('',#14396,#11422,#11423);
#8968=AXIS2_PLACEMENT_3D('',#14397,#11424,#11425);
#8969=AXIS2_PLACEMENT_3D('',#14398,#11426,#11427);
#8970=DIRECTION('axis',(0.,0.,1.));
#8971=DIRECTION('refdir',(1.,0.,0.));
#8972=DIRECTION('axis',(0.,0.,1.));
#8973=DIRECTION('refdir',(1.,0.,0.));
#8974=DIRECTION('axis',(0.,0.,1.));
#8975=DIRECTION('refdir',(1.,0.,0.));
#8976=DIRECTION('center_axis',(0.,0.,1.));
#8977=DIRECTION('ref_axis',(1.,0.,0.));
#8978=DIRECTION('center_axis',(0.,0.,1.));
#8979=DIRECTION('ref_axis',(1.,0.,0.));
#8980=DIRECTION('',(0.,0.,1.));
#8981=DIRECTION('center_axis',(0.,0.,-1.));
#8982=DIRECTION('ref_axis',(1.,0.,0.));
#8983=DIRECTION('center_axis',(0.,0.,1.));
#8984=DIRECTION('ref_axis',(1.,0.,0.));
#8985=DIRECTION('center_axis',(0.,0.,1.));
#8986=DIRECTION('ref_axis',(1.,0.,0.));
#8987=DIRECTION('',(0.,0.,1.));
#8988=DIRECTION('center_axis',(0.,0.,-1.));
#8989=DIRECTION('ref_axis',(1.,0.,0.));
#8990=DIRECTION('center_axis',(0.,0.,1.));
#8991=DIRECTION('ref_axis',(1.,0.,0.));
#8992=DIRECTION('center_axis',(0.,0.,1.));
#8993=DIRECTION('ref_axis',(1.,0.,0.));
#8994=DIRECTION('',(0.,0.,1.));
#8995=DIRECTION('center_axis',(0.,0.,-1.));
#8996=DIRECTION('ref_axis',(1.,0.,0.));
#8997=DIRECTION('center_axis',(0.,0.,1.));
#8998=DIRECTION('ref_axis',(1.,0.,0.));
#8999=DIRECTION('center_axis',(0.,0.,1.));
#9000=DIRECTION('ref_axis',(1.,0.,0.));
#9001=DIRECTION('',(0.,0.,1.));
#9002=DIRECTION('center_axis',(0.,0.,-1.));
#9003=DIRECTION('ref_axis',(1.,0.,0.));
#9004=DIRECTION('center_axis',(0.,1.,0.));
#9005=DIRECTION('ref_axis',(-1.,0.,0.));
#9006=DIRECTION('',(-1.,0.,0.));
#9007=DIRECTION('',(0.,0.,1.));
#9008=DIRECTION('',(-1.,0.,0.));
#9009=DIRECTION('',(0.,0.,1.));
#9010=DIRECTION('center_axis',(1.,0.,0.));
#9011=DIRECTION('ref_axis',(0.,1.,0.));
#9012=DIRECTION('',(0.,1.,0.));
#9013=DIRECTION('',(0.,1.,0.));
#9014=DIRECTION('',(0.,0.,1.));
#9015=DIRECTION('center_axis',(0.,-1.,0.));
#9016=DIRECTION('ref_axis',(1.,0.,0.));
#9017=DIRECTION('',(1.,0.,0.));
#9018=DIRECTION('',(1.,0.,0.));
#9019=DIRECTION('',(0.,0.,1.));
#9020=DIRECTION('center_axis',(-1.,0.,0.));
#9021=DIRECTION('ref_axis',(0.,-1.,0.));
#9022=DIRECTION('',(0.,-1.,0.));
#9023=DIRECTION('',(0.,-1.,0.));
#9024=DIRECTION('center_axis',(0.,0.,1.));
#9025=DIRECTION('ref_axis',(1.,0.,0.));
#9026=DIRECTION('center_axis',(0.,0.,1.));
#9027=DIRECTION('ref_axis',(1.,0.,0.));
#9028=DIRECTION('axis',(0.,0.,1.));
#9029=DIRECTION('refdir',(1.,0.,0.));
#9030=DIRECTION('center_axis',(0.,1.,0.));
#9031=DIRECTION('ref_axis',(-1.,0.,0.));
#9032=DIRECTION('',(-1.,0.,0.));
#9033=DIRECTION('',(0.,0.,1.));
#9034=DIRECTION('',(-1.,0.,0.));
#9035=DIRECTION('',(0.,0.,1.));
#9036=DIRECTION('center_axis',(1.,0.,0.));
#9037=DIRECTION('ref_axis',(0.,1.,0.));
#9038=DIRECTION('',(0.,1.,0.));
#9039=DIRECTION('',(0.,1.,0.));
#9040=DIRECTION('',(0.,0.,1.));
#9041=DIRECTION('center_axis',(0.,-1.,0.));
#9042=DIRECTION('ref_axis',(1.,0.,0.));
#9043=DIRECTION('',(1.,0.,0.));
#9044=DIRECTION('',(1.,0.,0.));
#9045=DIRECTION('',(0.,0.,1.));
#9046=DIRECTION('center_axis',(-1.,0.,0.));
#9047=DIRECTION('ref_axis',(0.,-1.,0.));
#9048=DIRECTION('',(0.,-1.,0.));
#9049=DIRECTION('',(0.,-1.,0.));
#9050=DIRECTION('center_axis',(0.,0.,1.));
#9051=DIRECTION('ref_axis',(1.,0.,0.));
#9052=DIRECTION('center_axis',(0.,0.,1.));
#9053=DIRECTION('ref_axis',(1.,0.,0.));
#9054=DIRECTION('axis',(0.,0.,1.));
#9055=DIRECTION('refdir',(1.,0.,0.));
#9056=DIRECTION('center_axis',(0.,1.,0.));
#9057=DIRECTION('ref_axis',(-1.,0.,0.));
#9058=DIRECTION('',(-1.,0.,0.));
#9059=DIRECTION('',(0.,0.,1.));
#9060=DIRECTION('',(-1.,0.,0.));
#9061=DIRECTION('',(0.,0.,1.));
#9062=DIRECTION('center_axis',(1.,0.,0.));
#9063=DIRECTION('ref_axis',(0.,1.,0.));
#9064=DIRECTION('',(0.,1.,0.));
#9065=DIRECTION('',(0.,1.,0.));
#9066=DIRECTION('',(0.,0.,1.));
#9067=DIRECTION('center_axis',(0.,-1.,0.));
#9068=DIRECTION('ref_axis',(1.,0.,0.));
#9069=DIRECTION('',(1.,0.,0.));
#9070=DIRECTION('',(1.,0.,0.));
#9071=DIRECTION('',(0.,0.,1.));
#9072=DIRECTION('center_axis',(-1.,0.,0.));
#9073=DIRECTION('ref_axis',(0.,-1.,0.));
#9074=DIRECTION('',(0.,-1.,0.));
#9075=DIRECTION('',(0.,-1.,0.));
#9076=DIRECTION('center_axis',(0.,0.,1.));
#9077=DIRECTION('ref_axis',(1.,0.,0.));
#9078=DIRECTION('center_axis',(0.,0.,1.));
#9079=DIRECTION('ref_axis',(1.,0.,0.));
#9080=DIRECTION('axis',(0.,0.,1.));
#9081=DIRECTION('refdir',(1.,0.,0.));
#9082=DIRECTION('center_axis',(1.,0.,0.));
#9083=DIRECTION('ref_axis',(0.,0.,-1.));
#9084=DIRECTION('center_axis',(1.,0.,0.));
#9085=DIRECTION('ref_axis',(0.,0.,-1.));
#9086=DIRECTION('',(1.,0.,0.));
#9087=DIRECTION('center_axis',(1.,0.,0.));
#9088=DIRECTION('ref_axis',(0.,0.,-1.));
#9089=DIRECTION('center_axis',(1.,0.,0.));
#9090=DIRECTION('ref_axis',(0.,0.,-1.));
#9091=DIRECTION('center_axis',(0.,1.,0.));
#9092=DIRECTION('ref_axis',(1.,0.,0.));
#9093=DIRECTION('center_axis',(0.,1.,0.));
#9094=DIRECTION('ref_axis',(1.,0.,0.));
#9095=DIRECTION('',(0.,1.,0.));
#9096=DIRECTION('center_axis',(0.,-1.,0.));
#9097=DIRECTION('ref_axis',(1.,0.,0.));
#9098=DIRECTION('center_axis',(0.,1.,0.));
#9099=DIRECTION('ref_axis',(1.,0.,0.));
#9100=DIRECTION('center_axis',(0.,1.,0.));
#9101=DIRECTION('ref_axis',(1.,0.,0.));
#9102=DIRECTION('',(0.,1.,0.));
#9103=DIRECTION('center_axis',(0.,-1.,0.));
#9104=DIRECTION('ref_axis',(1.,0.,0.));
#9105=DIRECTION('center_axis',(0.,1.,0.));
#9106=DIRECTION('ref_axis',(1.,0.,0.));
#9107=DIRECTION('center_axis',(0.,1.,0.));
#9108=DIRECTION('ref_axis',(1.,0.,0.));
#9109=DIRECTION('',(0.,1.,0.));
#9110=DIRECTION('center_axis',(0.,-1.,0.));
#9111=DIRECTION('ref_axis',(1.,0.,0.));
#9112=DIRECTION('center_axis',(0.,1.,0.));
#9113=DIRECTION('ref_axis',(1.,0.,0.));
#9114=DIRECTION('center_axis',(0.,1.,0.));
#9115=DIRECTION('ref_axis',(1.,0.,0.));
#9116=DIRECTION('',(0.,1.,0.));
#9117=DIRECTION('center_axis',(0.,-1.,0.));
#9118=DIRECTION('ref_axis',(1.,0.,0.));
#9119=DIRECTION('center_axis',(0.,1.,0.));
#9120=DIRECTION('ref_axis',(1.,0.,0.));
#9121=DIRECTION('center_axis',(0.,1.,0.));
#9122=DIRECTION('ref_axis',(1.,0.,0.));
#9123=DIRECTION('',(0.,1.,0.));
#9124=DIRECTION('center_axis',(0.,-1.,0.));
#9125=DIRECTION('ref_axis',(1.,0.,0.));
#9126=DIRECTION('center_axis',(0.,1.,0.));
#9127=DIRECTION('ref_axis',(1.,0.,0.));
#9128=DIRECTION('center_axis',(0.,1.,0.));
#9129=DIRECTION('ref_axis',(1.,0.,0.));
#9130=DIRECTION('',(0.,1.,0.));
#9131=DIRECTION('center_axis',(0.,-1.,0.));
#9132=DIRECTION('ref_axis',(1.,0.,0.));
#9133=DIRECTION('center_axis',(0.,1.,0.));
#9134=DIRECTION('ref_axis',(1.,0.,0.));
#9135=DIRECTION('center_axis',(0.,1.,0.));
#9136=DIRECTION('ref_axis',(1.,0.,0.));
#9137=DIRECTION('',(0.,1.,0.));
#9138=DIRECTION('center_axis',(0.,-1.,0.));
#9139=DIRECTION('ref_axis',(1.,0.,0.));
#9140=DIRECTION('center_axis',(0.,1.,0.));
#9141=DIRECTION('ref_axis',(1.,0.,0.));
#9142=DIRECTION('center_axis',(0.,1.,0.));
#9143=DIRECTION('ref_axis',(1.,0.,0.));
#9144=DIRECTION('',(0.,1.,0.));
#9145=DIRECTION('center_axis',(0.,-1.,0.));
#9146=DIRECTION('ref_axis',(1.,0.,0.));
#9147=DIRECTION('center_axis',(0.,0.,1.));
#9148=DIRECTION('ref_axis',(1.,0.,0.));
#9149=DIRECTION('center_axis',(0.,0.,1.));
#9150=DIRECTION('ref_axis',(1.,0.,0.));
#9151=DIRECTION('',(0.,0.,1.));
#9152=DIRECTION('center_axis',(0.,0.,-1.));
#9153=DIRECTION('ref_axis',(1.,0.,0.));
#9154=DIRECTION('center_axis',(0.,0.,1.));
#9155=DIRECTION('ref_axis',(1.,0.,0.));
#9156=DIRECTION('center_axis',(0.,0.,1.));
#9157=DIRECTION('ref_axis',(1.,0.,0.));
#9158=DIRECTION('',(0.,0.,1.));
#9159=DIRECTION('center_axis',(0.,0.,-1.));
#9160=DIRECTION('ref_axis',(1.,0.,0.));
#9161=DIRECTION('center_axis',(0.,0.,1.));
#9162=DIRECTION('ref_axis',(1.,0.,0.));
#9163=DIRECTION('center_axis',(0.,0.,1.));
#9164=DIRECTION('ref_axis',(1.,0.,0.));
#9165=DIRECTION('',(0.,0.,1.));
#9166=DIRECTION('center_axis',(0.,0.,-1.));
#9167=DIRECTION('ref_axis',(1.,0.,0.));
#9168=DIRECTION('center_axis',(0.,0.,1.));
#9169=DIRECTION('ref_axis',(1.,0.,0.));
#9170=DIRECTION('center_axis',(0.,0.,1.));
#9171=DIRECTION('ref_axis',(1.,0.,0.));
#9172=DIRECTION('',(0.,0.,1.));
#9173=DIRECTION('center_axis',(0.,0.,-1.));
#9174=DIRECTION('ref_axis',(1.,0.,0.));
#9175=DIRECTION('center_axis',(0.,0.,1.));
#9176=DIRECTION('ref_axis',(1.,0.,0.));
#9177=DIRECTION('',(0.,-1.,0.));
#9178=DIRECTION('',(-1.,0.,0.));
#9179=DIRECTION('',(0.,1.,0.));
#9180=DIRECTION('',(-1.,0.,0.));
#9181=DIRECTION('',(0.,1.,0.));
#9182=DIRECTION('',(1.,0.,0.));
#9183=DIRECTION('',(0.,1.,0.));
#9184=DIRECTION('',(-1.,0.,0.));
#9185=DIRECTION('center_axis',(-1.,0.,0.));
#9186=DIRECTION('ref_axis',(0.,0.,1.));
#9187=DIRECTION('',(0.,0.,-1.));
#9188=DIRECTION('',(0.,0.,1.));
#9189=DIRECTION('',(0.,1.,0.));
#9190=DIRECTION('center_axis',(0.,0.,-1.));
#9191=DIRECTION('ref_axis',(-1.,0.,0.));
#9192=DIRECTION('',(1.,0.,0.));
#9193=DIRECTION('',(-1.,0.,0.));
#9194=DIRECTION('',(0.,1.,0.));
#9195=DIRECTION('center_axis',(1.,0.,0.));
#9196=DIRECTION('ref_axis',(0.,0.,-1.));
#9197=DIRECTION('',(0.,0.,1.));
#9198=DIRECTION('',(0.,0.,-1.));
#9199=DIRECTION('center_axis',(0.,1.,0.));
#9200=DIRECTION('ref_axis',(0.,0.,1.));
#9201=DIRECTION('center_axis',(0.,1.,0.));
#9202=DIRECTION('ref_axis',(-1.,0.,0.));
#9203=DIRECTION('',(0.,0.,1.));
#9204=DIRECTION('',(-1.,0.,0.));
#9205=DIRECTION('',(0.,0.,1.));
#9206=DIRECTION('center_axis',(1.,0.,0.));
#9207=DIRECTION('ref_axis',(0.,1.,0.));
#9208=DIRECTION('',(0.,1.,0.));
#9209=DIRECTION('',(0.,0.,1.));
#9210=DIRECTION('center_axis',(0.,-1.,0.));
#9211=DIRECTION('ref_axis',(1.,0.,0.));
#9212=DIRECTION('',(1.,0.,0.));
#9213=DIRECTION('',(0.,0.,1.));
#9214=DIRECTION('center_axis',(-1.,0.,0.));
#9215=DIRECTION('ref_axis',(0.,-1.,0.));
#9216=DIRECTION('',(0.,-1.,0.));
#9217=DIRECTION('center_axis',(0.,0.,1.));
#9218=DIRECTION('ref_axis',(1.,0.,0.));
#9219=DIRECTION('axis',(0.,0.,1.));
#9220=DIRECTION('refdir',(1.,0.,0.));
#9221=DIRECTION('center_axis',(0.,1.,0.));
#9222=DIRECTION('ref_axis',(1.,0.,0.));
#9223=DIRECTION('center_axis',(0.,1.,0.));
#9224=DIRECTION('ref_axis',(1.,0.,0.));
#9225=DIRECTION('',(0.,1.,0.));
#9226=DIRECTION('center_axis',(0.,1.,0.));
#9227=DIRECTION('ref_axis',(1.,0.,0.));
#9228=DIRECTION('center_axis',(0.,1.,0.));
#9229=DIRECTION('ref_axis',(1.,0.,0.));
#9230=DIRECTION('center_axis',(0.,1.,0.));
#9231=DIRECTION('ref_axis',(1.,0.,0.));
#9232=DIRECTION('center_axis',(0.,1.,0.));
#9233=DIRECTION('ref_axis',(1.,0.,0.));
#9234=DIRECTION('',(0.,1.,0.));
#9235=DIRECTION('center_axis',(0.,-1.,0.));
#9236=DIRECTION('ref_axis',(1.,0.,0.));
#9237=DIRECTION('center_axis',(0.,1.,0.));
#9238=DIRECTION('ref_axis',(1.,0.,0.));
#9239=DIRECTION('center_axis',(0.,1.,0.));
#9240=DIRECTION('ref_axis',(1.,0.,0.));
#9241=DIRECTION('',(0.,1.,0.));
#9242=DIRECTION('center_axis',(0.,-1.,0.));
#9243=DIRECTION('ref_axis',(1.,0.,0.));
#9244=DIRECTION('center_axis',(0.,1.,0.));
#9245=DIRECTION('ref_axis',(1.,0.,0.));
#9246=DIRECTION('center_axis',(0.,1.,0.));
#9247=DIRECTION('ref_axis',(1.,0.,0.));
#9248=DIRECTION('',(0.,1.,0.));
#9249=DIRECTION('center_axis',(0.,-1.,0.));
#9250=DIRECTION('ref_axis',(1.,0.,0.));
#9251=DIRECTION('center_axis',(0.,1.,0.));
#9252=DIRECTION('ref_axis',(1.,0.,0.));
#9253=DIRECTION('center_axis',(0.,1.,0.));
#9254=DIRECTION('ref_axis',(1.,0.,0.));
#9255=DIRECTION('center_axis',(0.,1.,0.));
#9256=DIRECTION('ref_axis',(1.,0.,0.));
#9257=DIRECTION('center_axis',(0.,1.,0.));
#9258=DIRECTION('ref_axis',(1.,0.,0.));
#9259=DIRECTION('center_axis',(0.,1.,0.));
#9260=DIRECTION('ref_axis',(1.,0.,0.));
#9261=DIRECTION('center_axis',(0.,-1.,0.));
#9262=DIRECTION('ref_axis',(1.,0.,0.));
#9263=DIRECTION('center_axis',(0.,1.,0.));
#9264=DIRECTION('ref_axis',(1.,0.,0.));
#9265=DIRECTION('',(0.,-1.,0.));
#9266=DIRECTION('center_axis',(0.,1.,0.));
#9267=DIRECTION('ref_axis',(1.,0.,0.));
#9268=DIRECTION('',(0.,-1.,0.));
#9269=DIRECTION('center_axis',(0.,1.,0.));
#9270=DIRECTION('ref_axis',(1.,0.,0.));
#9271=DIRECTION('center_axis',(0.,1.,0.));
#9272=DIRECTION('ref_axis',(1.,0.,0.));
#9273=DIRECTION('center_axis',(0.,1.,0.));
#9274=DIRECTION('ref_axis',(1.,0.,0.));
#9275=DIRECTION('',(0.,-1.,0.));
#9276=DIRECTION('center_axis',(0.,1.,0.));
#9277=DIRECTION('ref_axis',(1.,0.,0.));
#9278=DIRECTION('center_axis',(0.,1.,0.));
#9279=DIRECTION('ref_axis',(1.,0.,0.));
#9280=DIRECTION('axis',(0.,0.,1.));
#9281=DIRECTION('refdir',(1.,0.,0.));
#9282=DIRECTION('center_axis',(0.,1.,0.));
#9283=DIRECTION('ref_axis',(1.,0.,0.));
#9284=DIRECTION('center_axis',(0.,-1.,0.));
#9285=DIRECTION('ref_axis',(1.,0.,0.));
#9286=DIRECTION('',(0.,-1.,0.));
#9287=DIRECTION('center_axis',(0.,-1.,0.));
#9288=DIRECTION('ref_axis',(1.,0.,0.));
#9289=DIRECTION('center_axis',(0.,1.,0.));
#9290=DIRECTION('ref_axis',(1.,0.,0.));
#9291=DIRECTION('center_axis',(0.,1.,0.));
#9292=DIRECTION('ref_axis',(1.,0.,0.));
#9293=DIRECTION('',(0.,-1.,0.));
#9294=DIRECTION('center_axis',(0.,1.,0.));
#9295=DIRECTION('ref_axis',(1.,0.,0.));
#9296=DIRECTION('center_axis',(0.,1.,0.));
#9297=DIRECTION('ref_axis',(1.,0.,0.));
#9298=DIRECTION('center_axis',(0.,1.,0.));
#9299=DIRECTION('ref_axis',(1.,0.,0.));
#9300=DIRECTION('axis',(0.,0.,1.));
#9301=DIRECTION('refdir',(1.,0.,0.));
#9302=DIRECTION('center_axis',(0.,1.,0.));
#9303=DIRECTION('ref_axis',(1.,0.,0.));
#9304=DIRECTION('center_axis',(0.,-1.,0.));
#9305=DIRECTION('ref_axis',(1.,0.,0.));
#9306=DIRECTION('',(0.,-1.,0.));
#9307=DIRECTION('center_axis',(0.,-1.,0.));
#9308=DIRECTION('ref_axis',(1.,0.,0.));
#9309=DIRECTION('center_axis',(0.,1.,0.));
#9310=DIRECTION('ref_axis',(1.,0.,0.));
#9311=DIRECTION('center_axis',(0.,1.,0.));
#9312=DIRECTION('ref_axis',(1.,0.,0.));
#9313=DIRECTION('',(0.,-1.,0.));
#9314=DIRECTION('center_axis',(0.,1.,0.));
#9315=DIRECTION('ref_axis',(1.,0.,0.));
#9316=DIRECTION('center_axis',(0.,1.,0.));
#9317=DIRECTION('ref_axis',(1.,0.,0.));
#9318=DIRECTION('center_axis',(0.,1.,0.));
#9319=DIRECTION('ref_axis',(1.,0.,0.));
#9320=DIRECTION('axis',(0.,0.,1.));
#9321=DIRECTION('refdir',(1.,0.,0.));
#9322=DIRECTION('center_axis',(0.,1.,0.));
#9323=DIRECTION('ref_axis',(1.,0.,0.));
#9324=DIRECTION('center_axis',(0.,-1.,0.));
#9325=DIRECTION('ref_axis',(1.,0.,0.));
#9326=DIRECTION('',(0.,-1.,0.));
#9327=DIRECTION('center_axis',(0.,-1.,0.));
#9328=DIRECTION('ref_axis',(1.,0.,0.));
#9329=DIRECTION('center_axis',(0.,1.,0.));
#9330=DIRECTION('ref_axis',(1.,0.,0.));
#9331=DIRECTION('center_axis',(0.,1.,0.));
#9332=DIRECTION('ref_axis',(1.,0.,0.));
#9333=DIRECTION('',(0.,-1.,0.));
#9334=DIRECTION('center_axis',(0.,1.,0.));
#9335=DIRECTION('ref_axis',(1.,0.,0.));
#9336=DIRECTION('center_axis',(0.,1.,0.));
#9337=DIRECTION('ref_axis',(1.,0.,0.));
#9338=DIRECTION('center_axis',(0.,1.,0.));
#9339=DIRECTION('ref_axis',(1.,0.,0.));
#9340=DIRECTION('axis',(0.,0.,1.));
#9341=DIRECTION('refdir',(1.,0.,0.));
#9342=DIRECTION('center_axis',(0.,1.,0.));
#9343=DIRECTION('ref_axis',(1.,0.,0.));
#9344=DIRECTION('center_axis',(0.,-1.,0.));
#9345=DIRECTION('ref_axis',(1.,0.,0.));
#9346=DIRECTION('',(0.,-1.,0.));
#9347=DIRECTION('center_axis',(0.,-1.,0.));
#9348=DIRECTION('ref_axis',(1.,0.,0.));
#9349=DIRECTION('center_axis',(0.,1.,0.));
#9350=DIRECTION('ref_axis',(1.,0.,0.));
#9351=DIRECTION('center_axis',(0.,1.,0.));
#9352=DIRECTION('ref_axis',(1.,0.,0.));
#9353=DIRECTION('',(0.,-1.,0.));
#9354=DIRECTION('center_axis',(0.,1.,0.));
#9355=DIRECTION('ref_axis',(1.,0.,0.));
#9356=DIRECTION('center_axis',(0.,1.,0.));
#9357=DIRECTION('ref_axis',(1.,0.,0.));
#9358=DIRECTION('center_axis',(0.,1.,0.));
#9359=DIRECTION('ref_axis',(1.,0.,0.));
#9360=DIRECTION('axis',(0.,0.,1.));
#9361=DIRECTION('refdir',(1.,0.,0.));
#9362=DIRECTION('center_axis',(0.,1.,0.));
#9363=DIRECTION('ref_axis',(1.,0.,0.));
#9364=DIRECTION('center_axis',(0.,1.,0.));
#9365=DIRECTION('ref_axis',(1.,0.,0.));
#9366=DIRECTION('',(0.,1.,0.));
#9367=DIRECTION('center_axis',(0.,1.,0.));
#9368=DIRECTION('ref_axis',(1.,0.,0.));
#9369=DIRECTION('center_axis',(0.,1.,0.));
#9370=DIRECTION('ref_axis',(1.,0.,0.));
#9371=DIRECTION('center_axis',(0.,1.,0.));
#9372=DIRECTION('ref_axis',(1.,0.,0.));
#9373=DIRECTION('center_axis',(0.,1.,0.));
#9374=DIRECTION('ref_axis',(1.,0.,0.));
#9375=DIRECTION('',(0.,1.,0.));
#9376=DIRECTION('center_axis',(0.,-1.,0.));
#9377=DIRECTION('ref_axis',(1.,0.,0.));
#9378=DIRECTION('center_axis',(0.,1.,0.));
#9379=DIRECTION('ref_axis',(1.,0.,0.));
#9380=DIRECTION('center_axis',(0.,1.,0.));
#9381=DIRECTION('ref_axis',(1.,0.,0.));
#9382=DIRECTION('',(0.,1.,0.));
#9383=DIRECTION('center_axis',(0.,-1.,0.));
#9384=DIRECTION('ref_axis',(1.,0.,0.));
#9385=DIRECTION('center_axis',(0.,1.,0.));
#9386=DIRECTION('ref_axis',(1.,0.,0.));
#9387=DIRECTION('center_axis',(0.,1.,0.));
#9388=DIRECTION('ref_axis',(1.,0.,0.));
#9389=DIRECTION('',(0.,1.,0.));
#9390=DIRECTION('center_axis',(0.,-1.,0.));
#9391=DIRECTION('ref_axis',(1.,0.,0.));
#9392=DIRECTION('center_axis',(0.,1.,0.));
#9393=DIRECTION('ref_axis',(1.,0.,0.));
#9394=DIRECTION('center_axis',(0.,1.,0.));
#9395=DIRECTION('ref_axis',(1.,0.,0.));
#9396=DIRECTION('center_axis',(0.,1.,0.));
#9397=DIRECTION('ref_axis',(1.,0.,0.));
#9398=DIRECTION('center_axis',(0.,1.,0.));
#9399=DIRECTION('ref_axis',(1.,0.,0.));
#9400=DIRECTION('center_axis',(0.,1.,0.));
#9401=DIRECTION('ref_axis',(1.,0.,0.));
#9402=DIRECTION('center_axis',(0.,-1.,0.));
#9403=DIRECTION('ref_axis',(1.,0.,0.));
#9404=DIRECTION('center_axis',(0.,1.,0.));
#9405=DIRECTION('ref_axis',(1.,0.,0.));
#9406=DIRECTION('',(0.,-1.,0.));
#9407=DIRECTION('center_axis',(0.,1.,0.));
#9408=DIRECTION('ref_axis',(1.,0.,0.));
#9409=DIRECTION('',(0.,-1.,0.));
#9410=DIRECTION('center_axis',(0.,1.,0.));
#9411=DIRECTION('ref_axis',(1.,0.,0.));
#9412=DIRECTION('center_axis',(0.,1.,0.));
#9413=DIRECTION('ref_axis',(1.,0.,0.));
#9414=DIRECTION('center_axis',(0.,1.,0.));
#9415=DIRECTION('ref_axis',(1.,0.,0.));
#9416=DIRECTION('',(0.,-1.,0.));
#9417=DIRECTION('center_axis',(0.,1.,0.));
#9418=DIRECTION('ref_axis',(1.,0.,0.));
#9419=DIRECTION('center_axis',(0.,1.,0.));
#9420=DIRECTION('ref_axis',(1.,0.,0.));
#9421=DIRECTION('axis',(0.,0.,1.));
#9422=DIRECTION('refdir',(1.,0.,0.));
#9423=DIRECTION('center_axis',(0.,1.,0.));
#9424=DIRECTION('ref_axis',(1.,0.,0.));
#9425=DIRECTION('center_axis',(0.,-1.,0.));
#9426=DIRECTION('ref_axis',(1.,0.,0.));
#9427=DIRECTION('',(0.,-1.,0.));
#9428=DIRECTION('center_axis',(0.,-1.,0.));
#9429=DIRECTION('ref_axis',(1.,0.,0.));
#9430=DIRECTION('center_axis',(0.,1.,0.));
#9431=DIRECTION('ref_axis',(1.,0.,0.));
#9432=DIRECTION('center_axis',(0.,1.,0.));
#9433=DIRECTION('ref_axis',(1.,0.,0.));
#9434=DIRECTION('',(0.,-1.,0.));
#9435=DIRECTION('center_axis',(0.,1.,0.));
#9436=DIRECTION('ref_axis',(1.,0.,0.));
#9437=DIRECTION('center_axis',(0.,1.,0.));
#9438=DIRECTION('ref_axis',(1.,0.,0.));
#9439=DIRECTION('center_axis',(0.,1.,0.));
#9440=DIRECTION('ref_axis',(1.,0.,0.));
#9441=DIRECTION('axis',(0.,0.,1.));
#9442=DIRECTION('refdir',(1.,0.,0.));
#9443=DIRECTION('center_axis',(0.,1.,0.));
#9444=DIRECTION('ref_axis',(1.,0.,0.));
#9445=DIRECTION('center_axis',(0.,-1.,0.));
#9446=DIRECTION('ref_axis',(1.,0.,0.));
#9447=DIRECTION('',(0.,-1.,0.));
#9448=DIRECTION('center_axis',(0.,-1.,0.));
#9449=DIRECTION('ref_axis',(1.,0.,0.));
#9450=DIRECTION('center_axis',(0.,1.,0.));
#9451=DIRECTION('ref_axis',(1.,0.,0.));
#9452=DIRECTION('center_axis',(0.,1.,0.));
#9453=DIRECTION('ref_axis',(1.,0.,0.));
#9454=DIRECTION('',(0.,-1.,0.));
#9455=DIRECTION('center_axis',(0.,1.,0.));
#9456=DIRECTION('ref_axis',(1.,0.,0.));
#9457=DIRECTION('center_axis',(0.,1.,0.));
#9458=DIRECTION('ref_axis',(1.,0.,0.));
#9459=DIRECTION('center_axis',(0.,1.,0.));
#9460=DIRECTION('ref_axis',(1.,0.,0.));
#9461=DIRECTION('axis',(0.,0.,1.));
#9462=DIRECTION('refdir',(1.,0.,0.));
#9463=DIRECTION('center_axis',(0.,1.,0.));
#9464=DIRECTION('ref_axis',(1.,0.,0.));
#9465=DIRECTION('center_axis',(0.,-1.,0.));
#9466=DIRECTION('ref_axis',(1.,0.,0.));
#9467=DIRECTION('',(0.,-1.,0.));
#9468=DIRECTION('center_axis',(0.,-1.,0.));
#9469=DIRECTION('ref_axis',(1.,0.,0.));
#9470=DIRECTION('center_axis',(0.,1.,0.));
#9471=DIRECTION('ref_axis',(1.,0.,0.));
#9472=DIRECTION('center_axis',(0.,1.,0.));
#9473=DIRECTION('ref_axis',(1.,0.,0.));
#9474=DIRECTION('',(0.,-1.,0.));
#9475=DIRECTION('center_axis',(0.,1.,0.));
#9476=DIRECTION('ref_axis',(1.,0.,0.));
#9477=DIRECTION('center_axis',(0.,1.,0.));
#9478=DIRECTION('ref_axis',(1.,0.,0.));
#9479=DIRECTION('center_axis',(0.,1.,0.));
#9480=DIRECTION('ref_axis',(1.,0.,0.));
#9481=DIRECTION('axis',(0.,0.,1.));
#9482=DIRECTION('refdir',(1.,0.,0.));
#9483=DIRECTION('center_axis',(0.,1.,0.));
#9484=DIRECTION('ref_axis',(1.,0.,0.));
#9485=DIRECTION('center_axis',(0.,-1.,0.));
#9486=DIRECTION('ref_axis',(1.,0.,0.));
#9487=DIRECTION('',(0.,-1.,0.));
#9488=DIRECTION('center_axis',(0.,-1.,0.));
#9489=DIRECTION('ref_axis',(1.,0.,0.));
#9490=DIRECTION('center_axis',(0.,1.,0.));
#9491=DIRECTION('ref_axis',(1.,0.,0.));
#9492=DIRECTION('center_axis',(0.,1.,0.));
#9493=DIRECTION('ref_axis',(1.,0.,0.));
#9494=DIRECTION('',(0.,-1.,0.));
#9495=DIRECTION('center_axis',(0.,1.,0.));
#9496=DIRECTION('ref_axis',(1.,0.,0.));
#9497=DIRECTION('center_axis',(0.,1.,0.));
#9498=DIRECTION('ref_axis',(1.,0.,0.));
#9499=DIRECTION('center_axis',(0.,1.,0.));
#9500=DIRECTION('ref_axis',(1.,0.,0.));
#9501=DIRECTION('axis',(0.,0.,1.));
#9502=DIRECTION('refdir',(1.,0.,0.));
#9503=DIRECTION('center_axis',(1.,0.,0.));
#9504=DIRECTION('ref_axis',(0.,0.,-1.));
#9505=DIRECTION('center_axis',(1.,0.,0.));
#9506=DIRECTION('ref_axis',(0.,0.,-1.));
#9507=DIRECTION('',(1.,0.,0.));
#9508=DIRECTION('center_axis',(-1.,0.,0.));
#9509=DIRECTION('ref_axis',(0.,0.,-1.));
#9510=DIRECTION('center_axis',(0.,0.,1.));
#9511=DIRECTION('ref_axis',(1.,0.,0.));
#9512=DIRECTION('center_axis',(0.,0.,1.));
#9513=DIRECTION('ref_axis',(1.,0.,0.));
#9514=DIRECTION('',(0.,0.,1.));
#9515=DIRECTION('center_axis',(0.,0.,-1.));
#9516=DIRECTION('ref_axis',(1.,0.,0.));
#9517=DIRECTION('center_axis',(-1.,0.,0.));
#9518=DIRECTION('ref_axis',(0.,0.,1.));
#9519=DIRECTION('',(0.,1.,0.));
#9520=DIRECTION('',(0.,0.,-1.));
#9521=DIRECTION('',(0.,1.,0.));
#9522=DIRECTION('',(0.,0.,1.));
#9523=DIRECTION('center_axis',(0.,0.,1.));
#9524=DIRECTION('ref_axis',(1.,0.,0.));
#9525=DIRECTION('',(-1.,0.,0.));
#9526=DIRECTION('',(0.,1.,0.));
#9527=DIRECTION('',(1.,0.,0.));
#9528=DIRECTION('center_axis',(0.,-1.,0.));
#9529=DIRECTION('ref_axis',(1.,0.,0.));
#9530=DIRECTION('',(-1.,0.,0.));
#9531=DIRECTION('',(0.,0.,1.));
#9532=DIRECTION('',(1.,0.,0.));
#9533=DIRECTION('',(0.,0.,1.));
#9534=DIRECTION('',(1.,0.,0.));
#9535=DIRECTION('',(0.,0.,1.));
#9536=DIRECTION('center_axis',(0.,0.,1.));
#9537=DIRECTION('ref_axis',(1.,0.,0.));
#9538=DIRECTION('',(1.,0.,0.));
#9539=DIRECTION('',(0.,1.,0.));
#9540=DIRECTION('center_axis',(0.,1.,0.));
#9541=DIRECTION('ref_axis',(0.,0.,1.));
#9542=DIRECTION('',(-1.,0.,0.));
#9543=DIRECTION('',(0.,0.,-1.));
#9544=DIRECTION('',(0.,0.,-1.));
#9545=DIRECTION('center_axis',(1.,0.,0.));
#9546=DIRECTION('ref_axis',(0.,0.,-1.));
#9547=DIRECTION('',(0.,1.,0.));
#9548=DIRECTION('center_axis',(-1.,0.,0.));
#9549=DIRECTION('ref_axis',(0.,-1.,0.));
#9550=DIRECTION('',(0.,-1.,0.));
#9551=DIRECTION('',(0.,-1.,0.));
#9552=DIRECTION('',(0.,0.,1.));
#9553=DIRECTION('center_axis',(0.,1.,0.));
#9554=DIRECTION('ref_axis',(-1.,0.,0.));
#9555=DIRECTION('',(-1.,0.,0.));
#9556=DIRECTION('',(-1.,0.,0.));
#9557=DIRECTION('',(0.,0.,1.));
#9558=DIRECTION('center_axis',(1.,0.,0.));
#9559=DIRECTION('ref_axis',(0.,1.,0.));
#9560=DIRECTION('',(0.,1.,0.));
#9561=DIRECTION('',(0.,1.,0.));
#9562=DIRECTION('center_axis',(0.,0.,1.));
#9563=DIRECTION('ref_axis',(1.,0.,0.));
#9564=DIRECTION('center_axis',(0.,0.,1.));
#9565=DIRECTION('ref_axis',(1.,0.,0.));
#9566=DIRECTION('axis',(0.,0.,1.));
#9567=DIRECTION('refdir',(1.,0.,0.));
#9568=DIRECTION('center_axis',(1.,0.,0.));
#9569=DIRECTION('ref_axis',(0.,0.,-1.));
#9570=DIRECTION('center_axis',(1.,0.,0.));
#9571=DIRECTION('ref_axis',(0.,0.,-1.));
#9572=DIRECTION('',(-1.,0.,0.));
#9573=DIRECTION('center_axis',(1.,0.,0.));
#9574=DIRECTION('ref_axis',(0.,0.,-1.));
#9575=DIRECTION('center_axis',(1.,0.,0.));
#9576=DIRECTION('ref_axis',(0.,0.,-1.));
#9577=DIRECTION('center_axis',(1.,0.,0.));
#9578=DIRECTION('ref_axis',(0.,0.,-1.));
#9579=DIRECTION('center_axis',(1.,0.,0.));
#9580=DIRECTION('ref_axis',(0.,0.,-1.));
#9581=DIRECTION('',(0.,0.996867356793964,0.0790915479594076));
#9582=DIRECTION('center_axis',(0.000135869568084146,-0.0790915472293713,
0.99686734759261));
#9583=DIRECTION('ref_axis',(-0.997148648532906,-0.0752365903152447,-0.00583337010099326));
#9584=DIRECTION('center_axis',(0.000135869568084146,-0.0790915472293713,
0.99686734759261));
#9585=DIRECTION('ref_axis',(-0.997148648532906,-0.0752365903152447,-0.00583337010099326));
#9586=DIRECTION('center_axis',(0.,0.,1.));
#9587=DIRECTION('ref_axis',(1.,0.,0.));
#9588=DIRECTION('center_axis',(0.,0.,1.));
#9589=DIRECTION('ref_axis',(1.,0.,0.));
#9590=DIRECTION('',(0.,0.,-1.));
#9591=DIRECTION('center_axis',(0.,0.,1.));
#9592=DIRECTION('ref_axis',(1.,0.,0.));
#9593=DIRECTION('center_axis',(0.,0.,1.));
#9594=DIRECTION('ref_axis',(1.,0.,0.));
#9595=DIRECTION('center_axis',(0.,0.,1.));
#9596=DIRECTION('ref_axis',(1.,0.,0.));
#9597=DIRECTION('',(0.999998524451305,-0.00171787520298126,0.));
#9598=DIRECTION('center_axis',(-0.000135869608335795,-0.0790915472892204,
0.996867347587856));
#9599=DIRECTION('ref_axis',(1.07799071550222E-5,-0.996867356847137,-0.0790915465545881));
#9600=DIRECTION('center_axis',(-0.000135869608335795,-0.0790915472892204,
0.996867347587856));
#9601=DIRECTION('ref_axis',(1.07799071550222E-5,-0.996867356847137,-0.0790915465545882));
#9602=DIRECTION('axis',(0.,0.,1.));
#9603=DIRECTION('refdir',(1.,0.,0.));
#9604=DIRECTION('center_axis',(0.866025403784439,0.,-0.5));
#9605=DIRECTION('ref_axis',(0.5,0.,0.866025403784439));
#9606=DIRECTION('',(-0.5,0.,-0.866025403784439));
#9607=DIRECTION('',(0.,-1.,0.));
#9608=DIRECTION('',(0.5,0.,0.866025403784439));
#9609=DIRECTION('',(0.,-1.,0.));
#9610=DIRECTION('center_axis',(1.20185167898973E-16,0.,-1.));
#9611=DIRECTION('ref_axis',(1.,0.,1.20185167898973E-16));
#9612=DIRECTION('',(-1.,0.,-1.20185167898973E-16));
#9613=DIRECTION('',(0.,-1.,0.));
#9614=DIRECTION('',(1.,0.,1.20185167898973E-16));
#9615=DIRECTION('center_axis',(-0.866025403784439,0.,-0.5));
#9616=DIRECTION('ref_axis',(0.5,0.,-0.866025403784439));
#9617=DIRECTION('',(-0.5,0.,0.866025403784439));
#9618=DIRECTION('',(0.,-1.,0.));
#9619=DIRECTION('',(0.5,0.,-0.866025403784439));
#9620=DIRECTION('center_axis',(-0.866025403784439,0.,0.5));
#9621=DIRECTION('ref_axis',(-0.5,0.,-0.866025403784439));
#9622=DIRECTION('',(0.5,0.,0.866025403784439));
#9623=DIRECTION('',(0.,-1.,0.));
#9624=DIRECTION('',(-0.5,0.,-0.866025403784439));
#9625=DIRECTION('center_axis',(-2.40370335797945E-16,0.,1.));
#9626=DIRECTION('ref_axis',(-1.,0.,-2.40370335797945E-16));
#9627=DIRECTION('',(1.,0.,2.40370335797945E-16));
#9628=DIRECTION('',(0.,-1.,0.));
#9629=DIRECTION('',(-1.,0.,-2.40370335797945E-16));
#9630=DIRECTION('center_axis',(0.866025403784439,0.,0.5));
#9631=DIRECTION('ref_axis',(-0.5,0.,0.866025403784439));
#9632=DIRECTION('',(0.5,0.,-0.866025403784439));
#9633=DIRECTION('',(-0.5,0.,0.866025403784439));
#9634=DIRECTION('center_axis',(0.,1.,0.));
#9635=DIRECTION('ref_axis',(1.,0.,0.));
#9636=DIRECTION('center_axis',(0.,-1.,0.));
#9637=DIRECTION('ref_axis',(0.,0.,-1.));
#9638=DIRECTION('center_axis',(0.,1.,0.));
#9639=DIRECTION('ref_axis',(1.,0.,0.));
#9640=DIRECTION('center_axis',(0.,1.,0.));
#9641=DIRECTION('ref_axis',(1.,0.,0.));
#9642=DIRECTION('center_axis',(0.,1.,0.));
#9643=DIRECTION('ref_axis',(0.,0.,1.));
#9644=DIRECTION('center_axis',(0.,-1.,0.));
#9645=DIRECTION('ref_axis',(1.,0.,0.));
#9646=DIRECTION('center_axis',(0.,-1.,0.));
#9647=DIRECTION('ref_axis',(1.,0.,0.));
#9648=DIRECTION('center_axis',(0.,-1.,0.));
#9649=DIRECTION('ref_axis',(1.,0.,0.));
#9650=DIRECTION('',(0.707106781186548,0.707106781186547,8.65956056235493E-17));
#9651=DIRECTION('center_axis',(0.,-1.,0.));
#9652=DIRECTION('ref_axis',(1.,0.,0.));
#9653=DIRECTION('center_axis',(0.,-1.,0.));
#9654=DIRECTION('ref_axis',(1.,0.,0.));
#9655=DIRECTION('',(0.,1.,0.));
#9656=DIRECTION('center_axis',(0.,1.,0.));
#9657=DIRECTION('ref_axis',(1.,0.,0.));
#9658=DIRECTION('center_axis',(0.,-1.,0.));
#9659=DIRECTION('ref_axis',(1.,0.,0.));
#9660=DIRECTION('',(-0.707106781186547,0.707106781186548,-8.65956056235493E-17));
#9661=DIRECTION('center_axis',(0.,-1.,0.));
#9662=DIRECTION('ref_axis',(0.,0.,-1.));
#9663=DIRECTION('center_axis',(0.,-1.,0.));
#9664=DIRECTION('ref_axis',(1.,0.,0.));
#9665=DIRECTION('center_axis',(0.,1.,0.));
#9666=DIRECTION('ref_axis',(1.,0.,0.));
#9667=DIRECTION('center_axis',(0.,1.,0.));
#9668=DIRECTION('ref_axis',(1.,0.,0.));
#9669=DIRECTION('',(-0.447213595499958,0.894427190999916,-5.47678698264203E-17));
#9670=DIRECTION('center_axis',(0.,-1.,0.));
#9671=DIRECTION('ref_axis',(1.,0.,0.));
#9672=DIRECTION('',(0.,1.,0.));
#9673=DIRECTION('axis',(0.,0.,1.));
#9674=DIRECTION('refdir',(1.,0.,0.));
#9675=DIRECTION('axis',(0.,0.,1.));
#9676=DIRECTION('refdir',(1.,0.,0.));
#9677=DIRECTION('center_axis',(0.,1.,0.));
#9678=DIRECTION('ref_axis',(1.,0.,0.));
#9679=DIRECTION('center_axis',(0.,1.,0.));
#9680=DIRECTION('ref_axis',(1.,0.,0.));
#9681=DIRECTION('',(0.,1.,0.));
#9682=DIRECTION('center_axis',(0.,-1.,0.));
#9683=DIRECTION('ref_axis',(1.,0.,0.));
#9684=DIRECTION('center_axis',(0.,1.,0.));
#9685=DIRECTION('ref_axis',(1.,0.,0.));
#9686=DIRECTION('center_axis',(0.,1.,0.));
#9687=DIRECTION('ref_axis',(1.,0.,0.));
#9688=DIRECTION('',(0.,1.,0.));
#9689=DIRECTION('center_axis',(0.,-1.,0.));
#9690=DIRECTION('ref_axis',(1.,0.,0.));
#9691=DIRECTION('center_axis',(0.,1.,0.));
#9692=DIRECTION('ref_axis',(1.,0.,0.));
#9693=DIRECTION('center_axis',(0.,1.,0.));
#9694=DIRECTION('ref_axis',(1.,0.,0.));
#9695=DIRECTION('',(0.,1.,0.));
#9696=DIRECTION('center_axis',(0.,-1.,0.));
#9697=DIRECTION('ref_axis',(1.,0.,0.));
#9698=DIRECTION('center_axis',(0.,1.,0.));
#9699=DIRECTION('ref_axis',(1.,0.,0.));
#9700=DIRECTION('center_axis',(0.,1.,0.));
#9701=DIRECTION('ref_axis',(1.,0.,0.));
#9702=DIRECTION('',(0.,1.,0.));
#9703=DIRECTION('center_axis',(0.,-1.,0.));
#9704=DIRECTION('ref_axis',(1.,0.,0.));
#9705=DIRECTION('center_axis',(0.,1.,0.));
#9706=DIRECTION('ref_axis',(1.,0.,0.));
#9707=DIRECTION('center_axis',(0.,1.,0.));
#9708=DIRECTION('ref_axis',(1.,0.,0.));
#9709=DIRECTION('',(0.,1.,0.));
#9710=DIRECTION('center_axis',(0.,-1.,0.));
#9711=DIRECTION('ref_axis',(1.,0.,0.));
#9712=DIRECTION('center_axis',(0.,1.,0.));
#9713=DIRECTION('ref_axis',(1.,0.,0.));
#9714=DIRECTION('center_axis',(0.,1.,0.));
#9715=DIRECTION('ref_axis',(1.,0.,0.));
#9716=DIRECTION('',(0.,1.,0.));
#9717=DIRECTION('center_axis',(0.,-1.,0.));
#9718=DIRECTION('ref_axis',(1.,0.,0.));
#9719=DIRECTION('center_axis',(0.,1.,0.));
#9720=DIRECTION('ref_axis',(1.,0.,0.));
#9721=DIRECTION('center_axis',(0.,1.,0.));
#9722=DIRECTION('ref_axis',(1.,0.,0.));
#9723=DIRECTION('',(0.,1.,0.));
#9724=DIRECTION('center_axis',(0.,-1.,0.));
#9725=DIRECTION('ref_axis',(1.,0.,0.));
#9726=DIRECTION('center_axis',(0.,1.,0.));
#9727=DIRECTION('ref_axis',(1.,0.,0.));
#9728=DIRECTION('center_axis',(0.,1.,0.));
#9729=DIRECTION('ref_axis',(1.,0.,0.));
#9730=DIRECTION('',(0.,1.,0.));
#9731=DIRECTION('center_axis',(0.,-1.,0.));
#9732=DIRECTION('ref_axis',(1.,0.,0.));
#9733=DIRECTION('center_axis',(0.,1.,0.));
#9734=DIRECTION('ref_axis',(1.,0.,0.));
#9735=DIRECTION('center_axis',(0.,1.,0.));
#9736=DIRECTION('ref_axis',(1.,0.,0.));
#9737=DIRECTION('',(0.,1.,0.));
#9738=DIRECTION('center_axis',(0.,-1.,0.));
#9739=DIRECTION('ref_axis',(1.,0.,0.));
#9740=DIRECTION('center_axis',(0.,1.,0.));
#9741=DIRECTION('ref_axis',(1.,0.,0.));
#9742=DIRECTION('center_axis',(0.,1.,0.));
#9743=DIRECTION('ref_axis',(1.,0.,0.));
#9744=DIRECTION('',(0.,1.,0.));
#9745=DIRECTION('center_axis',(0.,-1.,0.));
#9746=DIRECTION('ref_axis',(1.,0.,0.));
#9747=DIRECTION('center_axis',(0.,1.,0.));
#9748=DIRECTION('ref_axis',(1.,0.,0.));
#9749=DIRECTION('',(0.,-1.,0.));
#9750=DIRECTION('center_axis',(0.,1.,0.));
#9751=DIRECTION('ref_axis',(1.,0.,0.));
#9752=DIRECTION('',(0.,1.,0.));
#9753=DIRECTION('center_axis',(0.,1.,0.));
#9754=DIRECTION('ref_axis',(1.,0.,0.));
#9755=DIRECTION('center_axis',(0.,0.,-1.));
#9756=DIRECTION('ref_axis',(-1.,0.,0.));
#9757=DIRECTION('',(1.,0.,0.));
#9758=DIRECTION('',(0.,-1.,0.));
#9759=DIRECTION('',(-1.,0.,0.));
#9760=DIRECTION('center_axis',(0.,1.,0.));
#9761=DIRECTION('ref_axis',(1.,0.,0.));
#9762=DIRECTION('',(-1.,0.,0.));
#9763=DIRECTION('center_axis',(0.,1.,0.));
#9764=DIRECTION('ref_axis',(1.,0.,0.));
#9765=DIRECTION('center_axis',(0.,0.,1.));
#9766=DIRECTION('ref_axis',(1.,0.,0.));
#9767=DIRECTION('',(1.,0.,0.));
#9768=DIRECTION('',(0.,1.,0.));
#9769=DIRECTION('center_axis',(0.,1.,0.));
#9770=DIRECTION('ref_axis',(-1.,0.,-1.22464679914735E-16));
#9771=DIRECTION('center_axis',(0.,1.,0.));
#9772=DIRECTION('ref_axis',(1.,0.,0.));
#9773=DIRECTION('center_axis',(0.,1.,0.));
#9774=DIRECTION('ref_axis',(1.,0.,0.));
#9775=DIRECTION('axis',(0.,0.,1.));
#9776=DIRECTION('refdir',(1.,0.,0.));
#9777=DIRECTION('center_axis',(0.,1.,0.));
#9778=DIRECTION('ref_axis',(1.,0.,0.));
#9779=DIRECTION('center_axis',(0.,-1.,0.));
#9780=DIRECTION('ref_axis',(1.,0.,0.));
#9781=DIRECTION('',(0.,-1.,0.));
#9782=DIRECTION('center_axis',(0.,-1.,0.));
#9783=DIRECTION('ref_axis',(1.,0.,0.));
#9784=DIRECTION('center_axis',(0.,1.,0.));
#9785=DIRECTION('ref_axis',(1.,0.,0.));
#9786=DIRECTION('center_axis',(0.,1.,0.));
#9787=DIRECTION('ref_axis',(1.,0.,0.));
#9788=DIRECTION('',(0.,-1.,0.));
#9789=DIRECTION('center_axis',(0.,1.,0.));
#9790=DIRECTION('ref_axis',(1.,0.,0.));
#9791=DIRECTION('center_axis',(0.,1.,0.));
#9792=DIRECTION('ref_axis',(1.,0.,0.));
#9793=DIRECTION('center_axis',(0.,1.,0.));
#9794=DIRECTION('ref_axis',(1.,0.,0.));
#9795=DIRECTION('axis',(0.,0.,1.));
#9796=DIRECTION('refdir',(1.,0.,0.));
#9797=DIRECTION('center_axis',(0.,1.,0.));
#9798=DIRECTION('ref_axis',(1.,0.,0.));
#9799=DIRECTION('center_axis',(0.,1.,0.));
#9800=DIRECTION('ref_axis',(1.,0.,0.));
#9801=DIRECTION('',(0.,1.,0.));
#9802=DIRECTION('center_axis',(0.,-1.,0.));
#9803=DIRECTION('ref_axis',(1.,0.,0.));
#9804=DIRECTION('center_axis',(0.,1.,0.));
#9805=DIRECTION('ref_axis',(1.,0.,0.));
#9806=DIRECTION('center_axis',(0.,1.,0.));
#9807=DIRECTION('ref_axis',(1.,0.,0.));
#9808=DIRECTION('',(0.,1.,0.));
#9809=DIRECTION('center_axis',(0.,-1.,0.));
#9810=DIRECTION('ref_axis',(1.,0.,0.));
#9811=DIRECTION('center_axis',(0.,1.,0.));
#9812=DIRECTION('ref_axis',(1.,0.,0.));
#9813=DIRECTION('center_axis',(0.,1.,0.));
#9814=DIRECTION('ref_axis',(1.,0.,0.));
#9815=DIRECTION('',(0.,1.,0.));
#9816=DIRECTION('center_axis',(0.,-1.,0.));
#9817=DIRECTION('ref_axis',(1.,0.,0.));
#9818=DIRECTION('center_axis',(0.,1.,0.));
#9819=DIRECTION('ref_axis',(1.,0.,0.));
#9820=DIRECTION('center_axis',(0.,1.,0.));
#9821=DIRECTION('ref_axis',(1.,0.,0.));
#9822=DIRECTION('',(0.,1.,0.));
#9823=DIRECTION('center_axis',(0.,-1.,0.));
#9824=DIRECTION('ref_axis',(1.,0.,0.));
#9825=DIRECTION('center_axis',(0.,1.,0.));
#9826=DIRECTION('ref_axis',(1.,0.,0.));
#9827=DIRECTION('center_axis',(0.,-1.,0.));
#9828=DIRECTION('ref_axis',(1.,0.,0.));
#9829=DIRECTION('',(0.,-1.,0.));
#9830=DIRECTION('center_axis',(0.,-1.,0.));
#9831=DIRECTION('ref_axis',(1.,0.,0.));
#9832=DIRECTION('center_axis',(0.,1.,0.));
#9833=DIRECTION('ref_axis',(1.,0.,0.));
#9834=DIRECTION('center_axis',(0.,1.,0.));
#9835=DIRECTION('ref_axis',(1.,0.,0.));
#9836=DIRECTION('',(0.,-1.,0.));
#9837=DIRECTION('center_axis',(0.,1.,0.));
#9838=DIRECTION('ref_axis',(1.,0.,0.));
#9839=DIRECTION('center_axis',(0.,1.,0.));
#9840=DIRECTION('ref_axis',(1.,0.,0.));
#9841=DIRECTION('center_axis',(0.,1.,0.));
#9842=DIRECTION('ref_axis',(1.,0.,0.));
#9843=DIRECTION('axis',(0.,0.,1.));
#9844=DIRECTION('refdir',(1.,0.,0.));
#9845=DIRECTION('center_axis',(0.,1.,0.));
#9846=DIRECTION('ref_axis',(1.,0.,0.));
#9847=DIRECTION('center_axis',(0.,1.,0.));
#9848=DIRECTION('ref_axis',(1.,0.,0.));
#9849=DIRECTION('',(0.,1.,0.));
#9850=DIRECTION('center_axis',(0.,-1.,0.));
#9851=DIRECTION('ref_axis',(1.,0.,0.));
#9852=DIRECTION('center_axis',(0.,1.,0.));
#9853=DIRECTION('ref_axis',(1.,0.,0.));
#9854=DIRECTION('center_axis',(0.,1.,0.));
#9855=DIRECTION('ref_axis',(1.,0.,0.));
#9856=DIRECTION('',(0.,1.,0.));
#9857=DIRECTION('center_axis',(0.,-1.,0.));
#9858=DIRECTION('ref_axis',(1.,0.,0.));
#9859=DIRECTION('center_axis',(0.,1.,0.));
#9860=DIRECTION('ref_axis',(1.,0.,0.));
#9861=DIRECTION('center_axis',(0.,1.,0.));
#9862=DIRECTION('ref_axis',(1.,0.,0.));
#9863=DIRECTION('',(0.,1.,0.));
#9864=DIRECTION('center_axis',(0.,-1.,0.));
#9865=DIRECTION('ref_axis',(1.,0.,0.));
#9866=DIRECTION('center_axis',(0.,1.,0.));
#9867=DIRECTION('ref_axis',(1.,0.,0.));
#9868=DIRECTION('center_axis',(0.,1.,0.));
#9869=DIRECTION('ref_axis',(1.,0.,0.));
#9870=DIRECTION('',(0.,1.,0.));
#9871=DIRECTION('center_axis',(0.,-1.,0.));
#9872=DIRECTION('ref_axis',(1.,0.,0.));
#9873=DIRECTION('center_axis',(0.,1.,0.));
#9874=DIRECTION('ref_axis',(1.,0.,0.));
#9875=DIRECTION('center_axis',(0.,-1.,0.));
#9876=DIRECTION('ref_axis',(1.,0.,0.));
#9877=DIRECTION('',(0.,-1.,0.));
#9878=DIRECTION('center_axis',(0.,-1.,0.));
#9879=DIRECTION('ref_axis',(1.,0.,0.));
#9880=DIRECTION('center_axis',(0.,1.,0.));
#9881=DIRECTION('ref_axis',(1.,0.,0.));
#9882=DIRECTION('center_axis',(0.,1.,0.));
#9883=DIRECTION('ref_axis',(1.,0.,0.));
#9884=DIRECTION('',(0.,-1.,0.));
#9885=DIRECTION('center_axis',(0.,1.,0.));
#9886=DIRECTION('ref_axis',(1.,0.,0.));
#9887=DIRECTION('center_axis',(0.,1.,0.));
#9888=DIRECTION('ref_axis',(1.,0.,0.));
#9889=DIRECTION('center_axis',(0.,1.,0.));
#9890=DIRECTION('ref_axis',(1.,0.,0.));
#9891=DIRECTION('axis',(0.,0.,1.));
#9892=DIRECTION('refdir',(1.,0.,0.));
#9893=DIRECTION('center_axis',(0.,1.,0.));
#9894=DIRECTION('ref_axis',(1.,0.,0.));
#9895=DIRECTION('center_axis',(0.,-1.,0.));
#9896=DIRECTION('ref_axis',(1.,0.,0.));
#9897=DIRECTION('',(0.,-1.,0.));
#9898=DIRECTION('center_axis',(0.,-1.,0.));
#9899=DIRECTION('ref_axis',(1.,0.,0.));
#9900=DIRECTION('center_axis',(0.,1.,0.));
#9901=DIRECTION('ref_axis',(1.,0.,0.));
#9902=DIRECTION('center_axis',(0.,1.,0.));
#9903=DIRECTION('ref_axis',(1.,0.,0.));
#9904=DIRECTION('',(0.,-1.,0.));
#9905=DIRECTION('center_axis',(0.,1.,0.));
#9906=DIRECTION('ref_axis',(1.,0.,0.));
#9907=DIRECTION('center_axis',(0.,1.,0.));
#9908=DIRECTION('ref_axis',(1.,0.,0.));
#9909=DIRECTION('center_axis',(0.,1.,0.));
#9910=DIRECTION('ref_axis',(1.,0.,0.));
#9911=DIRECTION('axis',(0.,0.,1.));
#9912=DIRECTION('refdir',(1.,0.,0.));
#9913=DIRECTION('center_axis',(0.,1.,0.));
#9914=DIRECTION('ref_axis',(1.,0.,0.));
#9915=DIRECTION('center_axis',(0.,1.,0.));
#9916=DIRECTION('ref_axis',(1.,0.,0.));
#9917=DIRECTION('',(0.,1.,0.));
#9918=DIRECTION('center_axis',(0.,-1.,0.));
#9919=DIRECTION('ref_axis',(1.,0.,0.));
#9920=DIRECTION('center_axis',(0.,1.,0.));
#9921=DIRECTION('ref_axis',(1.,0.,0.));
#9922=DIRECTION('center_axis',(0.,1.,0.));
#9923=DIRECTION('ref_axis',(1.,0.,0.));
#9924=DIRECTION('',(0.,1.,0.));
#9925=DIRECTION('center_axis',(0.,-1.,0.));
#9926=DIRECTION('ref_axis',(1.,0.,0.));
#9927=DIRECTION('center_axis',(0.,1.,0.));
#9928=DIRECTION('ref_axis',(1.,0.,0.));
#9929=DIRECTION('center_axis',(0.,1.,0.));
#9930=DIRECTION('ref_axis',(1.,0.,0.));
#9931=DIRECTION('',(0.,1.,0.));
#9932=DIRECTION('center_axis',(0.,-1.,0.));
#9933=DIRECTION('ref_axis',(1.,0.,0.));
#9934=DIRECTION('center_axis',(0.,1.,0.));
#9935=DIRECTION('ref_axis',(1.,0.,0.));
#9936=DIRECTION('center_axis',(0.,1.,0.));
#9937=DIRECTION('ref_axis',(1.,0.,0.));
#9938=DIRECTION('',(0.,1.,0.));
#9939=DIRECTION('center_axis',(0.,-1.,0.));
#9940=DIRECTION('ref_axis',(1.,0.,0.));
#9941=DIRECTION('center_axis',(0.,1.,0.));
#9942=DIRECTION('ref_axis',(1.,0.,0.));
#9943=DIRECTION('center_axis',(0.,-1.,0.));
#9944=DIRECTION('ref_axis',(1.,0.,0.));
#9945=DIRECTION('',(0.,-1.,0.));
#9946=DIRECTION('center_axis',(0.,-1.,0.));
#9947=DIRECTION('ref_axis',(1.,0.,0.));
#9948=DIRECTION('center_axis',(0.,1.,0.));
#9949=DIRECTION('ref_axis',(1.,0.,0.));
#9950=DIRECTION('center_axis',(0.,1.,0.));
#9951=DIRECTION('ref_axis',(1.,0.,0.));
#9952=DIRECTION('',(0.,-1.,0.));
#9953=DIRECTION('center_axis',(0.,1.,0.));
#9954=DIRECTION('ref_axis',(1.,0.,0.));
#9955=DIRECTION('center_axis',(0.,1.,0.));
#9956=DIRECTION('ref_axis',(1.,0.,0.));
#9957=DIRECTION('center_axis',(0.,1.,0.));
#9958=DIRECTION('ref_axis',(1.,0.,0.));
#9959=DIRECTION('axis',(0.,0.,1.));
#9960=DIRECTION('refdir',(1.,0.,0.));
#9961=DIRECTION('center_axis',(0.,1.,0.));
#9962=DIRECTION('ref_axis',(1.,0.,0.));
#9963=DIRECTION('center_axis',(0.,1.,0.));
#9964=DIRECTION('ref_axis',(1.,0.,0.));
#9965=DIRECTION('',(0.,1.,0.));
#9966=DIRECTION('center_axis',(0.,-1.,0.));
#9967=DIRECTION('ref_axis',(1.,0.,0.));
#9968=DIRECTION('center_axis',(0.,1.,0.));
#9969=DIRECTION('ref_axis',(1.,0.,0.));
#9970=DIRECTION('center_axis',(0.,1.,0.));
#9971=DIRECTION('ref_axis',(1.,0.,0.));
#9972=DIRECTION('',(0.,1.,0.));
#9973=DIRECTION('center_axis',(0.,-1.,0.));
#9974=DIRECTION('ref_axis',(1.,0.,0.));
#9975=DIRECTION('center_axis',(0.,1.,0.));
#9976=DIRECTION('ref_axis',(1.,0.,0.));
#9977=DIRECTION('center_axis',(0.,1.,0.));
#9978=DIRECTION('ref_axis',(1.,0.,0.));
#9979=DIRECTION('',(0.,1.,0.));
#9980=DIRECTION('center_axis',(0.,-1.,0.));
#9981=DIRECTION('ref_axis',(1.,0.,0.));
#9982=DIRECTION('center_axis',(0.,1.,0.));
#9983=DIRECTION('ref_axis',(1.,0.,0.));
#9984=DIRECTION('center_axis',(0.,1.,0.));
#9985=DIRECTION('ref_axis',(1.,0.,0.));
#9986=DIRECTION('',(0.,1.,0.));
#9987=DIRECTION('center_axis',(0.,-1.,0.));
#9988=DIRECTION('ref_axis',(1.,0.,0.));
#9989=DIRECTION('center_axis',(0.,1.,0.));
#9990=DIRECTION('ref_axis',(1.,0.,0.));
#9991=DIRECTION('center_axis',(0.,-1.,0.));
#9992=DIRECTION('ref_axis',(1.,0.,0.));
#9993=DIRECTION('',(0.,-1.,0.));
#9994=DIRECTION('center_axis',(0.,-1.,0.));
#9995=DIRECTION('ref_axis',(1.,0.,0.));
#9996=DIRECTION('center_axis',(0.,1.,0.));
#9997=DIRECTION('ref_axis',(1.,0.,0.));
#9998=DIRECTION('center_axis',(0.,1.,0.));
#9999=DIRECTION('ref_axis',(1.,0.,0.));
#10000=DIRECTION('',(0.,-1.,0.));
#10001=DIRECTION('center_axis',(0.,1.,0.));
#10002=DIRECTION('ref_axis',(1.,0.,0.));
#10003=DIRECTION('center_axis',(0.,1.,0.));
#10004=DIRECTION('ref_axis',(1.,0.,0.));
#10005=DIRECTION('center_axis',(0.,1.,0.));
#10006=DIRECTION('ref_axis',(1.,0.,0.));
#10007=DIRECTION('axis',(0.,0.,1.));
#10008=DIRECTION('refdir',(1.,0.,0.));
#10009=DIRECTION('center_axis',(1.,0.,0.));
#10010=DIRECTION('ref_axis',(0.,0.,-1.));
#10011=DIRECTION('center_axis',(1.,0.,0.));
#10012=DIRECTION('ref_axis',(0.,0.,-1.));
#10013=DIRECTION('',(1.,0.,0.));
#10014=DIRECTION('center_axis',(-1.,0.,0.));
#10015=DIRECTION('ref_axis',(0.,0.,-1.));
#10016=DIRECTION('center_axis',(0.,1.,0.));
#10017=DIRECTION('ref_axis',(-1.,0.,0.));
#10018=DIRECTION('',(-1.,0.,0.));
#10019=DIRECTION('',(0.,0.,1.));
#10020=DIRECTION('',(-1.,0.,0.));
#10021=DIRECTION('',(0.,0.,1.));
#10022=DIRECTION('center_axis',(1.,0.,0.));
#10023=DIRECTION('ref_axis',(0.,1.,0.));
#10024=DIRECTION('',(0.,1.,0.));
#10025=DIRECTION('',(0.,1.,0.));
#10026=DIRECTION('',(0.,0.,1.));
#10027=DIRECTION('center_axis',(0.,-1.,0.));
#10028=DIRECTION('ref_axis',(1.,0.,0.));
#10029=DIRECTION('',(1.,0.,0.));
#10030=DIRECTION('',(1.,0.,0.));
#10031=DIRECTION('',(0.,0.,1.));
#10032=DIRECTION('center_axis',(-1.,0.,0.));
#10033=DIRECTION('ref_axis',(0.,-1.,0.));
#10034=DIRECTION('',(0.,-1.,0.));
#10035=DIRECTION('',(0.,-1.,0.));
#10036=DIRECTION('center_axis',(0.,0.,1.));
#10037=DIRECTION('ref_axis',(1.,0.,0.));
#10038=DIRECTION('center_axis',(0.,0.,1.));
#10039=DIRECTION('ref_axis',(1.,0.,0.));
#10040=DIRECTION('axis',(0.,0.,1.));
#10041=DIRECTION('refdir',(1.,0.,0.));
#10042=DIRECTION('axis',(0.,0.,1.));
#10043=DIRECTION('refdir',(1.,0.,0.));
#10044=DIRECTION('center_axis',(0.,1.,0.));
#10045=DIRECTION('ref_axis',(1.,0.,0.));
#10046=DIRECTION('center_axis',(0.,1.,0.));
#10047=DIRECTION('ref_axis',(1.,0.,0.));
#10048=DIRECTION('',(0.,1.,0.));
#10049=DIRECTION('center_axis',(0.,-1.,0.));
#10050=DIRECTION('ref_axis',(1.,0.,0.));
#10051=DIRECTION('center_axis',(0.,1.,0.));
#10052=DIRECTION('ref_axis',(1.,0.,0.));
#10053=DIRECTION('center_axis',(0.,1.,0.));
#10054=DIRECTION('ref_axis',(1.,0.,0.));
#10055=DIRECTION('',(0.,1.,0.));
#10056=DIRECTION('center_axis',(0.,-1.,0.));
#10057=DIRECTION('ref_axis',(1.,0.,0.));
#10058=DIRECTION('center_axis',(0.,1.,0.));
#10059=DIRECTION('ref_axis',(1.,0.,0.));
#10060=DIRECTION('center_axis',(0.,1.,0.));
#10061=DIRECTION('ref_axis',(1.,0.,0.));
#10062=DIRECTION('',(0.,1.,0.));
#10063=DIRECTION('center_axis',(0.,-1.,0.));
#10064=DIRECTION('ref_axis',(1.,0.,0.));
#10065=DIRECTION('center_axis',(0.,1.,0.));
#10066=DIRECTION('ref_axis',(1.,0.,0.));
#10067=DIRECTION('center_axis',(0.,1.,0.));
#10068=DIRECTION('ref_axis',(1.,0.,0.));
#10069=DIRECTION('',(0.,1.,0.));
#10070=DIRECTION('center_axis',(0.,-1.,0.));
#10071=DIRECTION('ref_axis',(1.,0.,0.));
#10072=DIRECTION('center_axis',(0.,1.,0.));
#10073=DIRECTION('ref_axis',(1.,0.,0.));
#10074=DIRECTION('center_axis',(0.,1.,0.));
#10075=DIRECTION('ref_axis',(1.,0.,0.));
#10076=DIRECTION('',(0.,1.,0.));
#10077=DIRECTION('center_axis',(0.,-1.,0.));
#10078=DIRECTION('ref_axis',(1.,0.,0.));
#10079=DIRECTION('center_axis',(0.,1.,0.));
#10080=DIRECTION('ref_axis',(1.,0.,0.));
#10081=DIRECTION('center_axis',(0.,1.,0.));
#10082=DIRECTION('ref_axis',(1.,0.,0.));
#10083=DIRECTION('',(0.,1.,0.));
#10084=DIRECTION('center_axis',(0.,-1.,0.));
#10085=DIRECTION('ref_axis',(1.,0.,0.));
#10086=DIRECTION('center_axis',(0.,1.,0.));
#10087=DIRECTION('ref_axis',(1.,0.,0.));
#10088=DIRECTION('center_axis',(0.,1.,0.));
#10089=DIRECTION('ref_axis',(1.,0.,0.));
#10090=DIRECTION('',(0.,1.,0.));
#10091=DIRECTION('center_axis',(0.,-1.,0.));
#10092=DIRECTION('ref_axis',(1.,0.,0.));
#10093=DIRECTION('center_axis',(0.,1.,0.));
#10094=DIRECTION('ref_axis',(1.,0.,0.));
#10095=DIRECTION('center_axis',(0.,1.,0.));
#10096=DIRECTION('ref_axis',(1.,0.,0.));
#10097=DIRECTION('',(0.,1.,0.));
#10098=DIRECTION('center_axis',(0.,-1.,0.));
#10099=DIRECTION('ref_axis',(1.,0.,0.));
#10100=DIRECTION('center_axis',(0.,1.,0.));
#10101=DIRECTION('ref_axis',(1.,0.,0.));
#10102=DIRECTION('center_axis',(0.,1.,0.));
#10103=DIRECTION('ref_axis',(1.,0.,0.));
#10104=DIRECTION('',(0.,1.,0.));
#10105=DIRECTION('center_axis',(0.,-1.,0.));
#10106=DIRECTION('ref_axis',(1.,0.,0.));
#10107=DIRECTION('center_axis',(0.,1.,0.));
#10108=DIRECTION('ref_axis',(1.,0.,0.));
#10109=DIRECTION('center_axis',(0.,1.,0.));
#10110=DIRECTION('ref_axis',(1.,0.,0.));
#10111=DIRECTION('',(0.,1.,0.));
#10112=DIRECTION('center_axis',(0.,-1.,0.));
#10113=DIRECTION('ref_axis',(1.,0.,0.));
#10114=DIRECTION('center_axis',(0.,1.,0.));
#10115=DIRECTION('ref_axis',(1.,0.,0.));
#10116=DIRECTION('',(0.,-1.,0.));
#10117=DIRECTION('center_axis',(0.,1.,0.));
#10118=DIRECTION('ref_axis',(1.,0.,0.));
#10119=DIRECTION('',(0.,1.,0.));
#10120=DIRECTION('center_axis',(0.,1.,0.));
#10121=DIRECTION('ref_axis',(1.,0.,0.));
#10122=DIRECTION('center_axis',(0.,0.,-1.));
#10123=DIRECTION('ref_axis',(-1.,0.,0.));
#10124=DIRECTION('',(1.,0.,0.));
#10125=DIRECTION('',(0.,-1.,0.));
#10126=DIRECTION('',(-1.,0.,0.));
#10127=DIRECTION('center_axis',(0.,1.,0.));
#10128=DIRECTION('ref_axis',(1.,0.,0.));
#10129=DIRECTION('',(-1.,0.,0.));
#10130=DIRECTION('center_axis',(0.,1.,0.));
#10131=DIRECTION('ref_axis',(1.,0.,0.));
#10132=DIRECTION('center_axis',(0.,0.,1.));
#10133=DIRECTION('ref_axis',(1.,0.,0.));
#10134=DIRECTION('',(1.,0.,0.));
#10135=DIRECTION('',(0.,1.,0.));
#10136=DIRECTION('center_axis',(0.,1.,0.));
#10137=DIRECTION('ref_axis',(-1.,0.,-1.22464679914735E-16));
#10138=DIRECTION('center_axis',(0.,1.,0.));
#10139=DIRECTION('ref_axis',(1.,0.,0.));
#10140=DIRECTION('center_axis',(0.,1.,0.));
#10141=DIRECTION('ref_axis',(1.,0.,0.));
#10142=DIRECTION('axis',(0.,0.,1.));
#10143=DIRECTION('refdir',(1.,0.,0.));
#10144=DIRECTION('center_axis',(0.,1.,0.));
#10145=DIRECTION('ref_axis',(1.,0.,0.));
#10146=DIRECTION('center_axis',(0.,-1.,0.));
#10147=DIRECTION('ref_axis',(1.,0.,0.));
#10148=DIRECTION('',(0.,-1.,0.));
#10149=DIRECTION('center_axis',(0.,-1.,0.));
#10150=DIRECTION('ref_axis',(1.,0.,0.));
#10151=DIRECTION('center_axis',(0.,1.,0.));
#10152=DIRECTION('ref_axis',(1.,0.,0.));
#10153=DIRECTION('center_axis',(0.,1.,0.));
#10154=DIRECTION('ref_axis',(1.,0.,0.));
#10155=DIRECTION('',(0.,-1.,0.));
#10156=DIRECTION('center_axis',(0.,1.,0.));
#10157=DIRECTION('ref_axis',(1.,0.,0.));
#10158=DIRECTION('center_axis',(0.,1.,0.));
#10159=DIRECTION('ref_axis',(1.,0.,0.));
#10160=DIRECTION('center_axis',(0.,1.,0.));
#10161=DIRECTION('ref_axis',(1.,0.,0.));
#10162=DIRECTION('axis',(0.,0.,1.));
#10163=DIRECTION('refdir',(1.,0.,0.));
#10164=DIRECTION('center_axis',(0.,1.,0.));
#10165=DIRECTION('ref_axis',(1.,0.,0.));
#10166=DIRECTION('center_axis',(0.,1.,0.));
#10167=DIRECTION('ref_axis',(1.,0.,0.));
#10168=DIRECTION('',(0.,1.,0.));
#10169=DIRECTION('center_axis',(0.,-1.,0.));
#10170=DIRECTION('ref_axis',(1.,0.,0.));
#10171=DIRECTION('center_axis',(0.,1.,0.));
#10172=DIRECTION('ref_axis',(1.,0.,0.));
#10173=DIRECTION('center_axis',(0.,1.,0.));
#10174=DIRECTION('ref_axis',(1.,0.,0.));
#10175=DIRECTION('',(0.,1.,0.));
#10176=DIRECTION('center_axis',(0.,-1.,0.));
#10177=DIRECTION('ref_axis',(1.,0.,0.));
#10178=DIRECTION('center_axis',(0.,1.,0.));
#10179=DIRECTION('ref_axis',(1.,0.,0.));
#10180=DIRECTION('center_axis',(0.,1.,0.));
#10181=DIRECTION('ref_axis',(1.,0.,0.));
#10182=DIRECTION('',(0.,1.,0.));
#10183=DIRECTION('center_axis',(0.,-1.,0.));
#10184=DIRECTION('ref_axis',(1.,0.,0.));
#10185=DIRECTION('center_axis',(0.,1.,0.));
#10186=DIRECTION('ref_axis',(1.,0.,0.));
#10187=DIRECTION('center_axis',(0.,1.,0.));
#10188=DIRECTION('ref_axis',(1.,0.,0.));
#10189=DIRECTION('',(0.,1.,0.));
#10190=DIRECTION('center_axis',(0.,-1.,0.));
#10191=DIRECTION('ref_axis',(1.,0.,0.));
#10192=DIRECTION('center_axis',(0.,1.,0.));
#10193=DIRECTION('ref_axis',(1.,0.,0.));
#10194=DIRECTION('center_axis',(0.,-1.,0.));
#10195=DIRECTION('ref_axis',(1.,0.,0.));
#10196=DIRECTION('',(0.,-1.,0.));
#10197=DIRECTION('center_axis',(0.,-1.,0.));
#10198=DIRECTION('ref_axis',(1.,0.,0.));
#10199=DIRECTION('center_axis',(0.,1.,0.));
#10200=DIRECTION('ref_axis',(1.,0.,0.));
#10201=DIRECTION('center_axis',(0.,1.,0.));
#10202=DIRECTION('ref_axis',(1.,0.,0.));
#10203=DIRECTION('',(0.,-1.,0.));
#10204=DIRECTION('center_axis',(0.,1.,0.));
#10205=DIRECTION('ref_axis',(1.,0.,0.));
#10206=DIRECTION('center_axis',(0.,1.,0.));
#10207=DIRECTION('ref_axis',(1.,0.,0.));
#10208=DIRECTION('center_axis',(0.,1.,0.));
#10209=DIRECTION('ref_axis',(1.,0.,0.));
#10210=DIRECTION('axis',(0.,0.,1.));
#10211=DIRECTION('refdir',(1.,0.,0.));
#10212=DIRECTION('center_axis',(0.,1.,0.));
#10213=DIRECTION('ref_axis',(1.,0.,0.));
#10214=DIRECTION('center_axis',(0.,1.,0.));
#10215=DIRECTION('ref_axis',(1.,0.,0.));
#10216=DIRECTION('',(0.,1.,0.));
#10217=DIRECTION('center_axis',(0.,-1.,0.));
#10218=DIRECTION('ref_axis',(1.,0.,0.));
#10219=DIRECTION('center_axis',(0.,1.,0.));
#10220=DIRECTION('ref_axis',(1.,0.,0.));
#10221=DIRECTION('center_axis',(0.,1.,0.));
#10222=DIRECTION('ref_axis',(1.,0.,0.));
#10223=DIRECTION('',(0.,1.,0.));
#10224=DIRECTION('center_axis',(0.,-1.,0.));
#10225=DIRECTION('ref_axis',(1.,0.,0.));
#10226=DIRECTION('center_axis',(0.,1.,0.));
#10227=DIRECTION('ref_axis',(1.,0.,0.));
#10228=DIRECTION('center_axis',(0.,1.,0.));
#10229=DIRECTION('ref_axis',(1.,0.,0.));
#10230=DIRECTION('',(0.,1.,0.));
#10231=DIRECTION('center_axis',(0.,-1.,0.));
#10232=DIRECTION('ref_axis',(1.,0.,0.));
#10233=DIRECTION('center_axis',(0.,1.,0.));
#10234=DIRECTION('ref_axis',(1.,0.,0.));
#10235=DIRECTION('center_axis',(0.,1.,0.));
#10236=DIRECTION('ref_axis',(1.,0.,0.));
#10237=DIRECTION('',(0.,1.,0.));
#10238=DIRECTION('center_axis',(0.,-1.,0.));
#10239=DIRECTION('ref_axis',(1.,0.,0.));
#10240=DIRECTION('center_axis',(0.,1.,0.));
#10241=DIRECTION('ref_axis',(1.,0.,0.));
#10242=DIRECTION('center_axis',(0.,-1.,0.));
#10243=DIRECTION('ref_axis',(1.,0.,0.));
#10244=DIRECTION('',(0.,-1.,0.));
#10245=DIRECTION('center_axis',(0.,-1.,0.));
#10246=DIRECTION('ref_axis',(1.,0.,0.));
#10247=DIRECTION('center_axis',(0.,1.,0.));
#10248=DIRECTION('ref_axis',(1.,0.,0.));
#10249=DIRECTION('center_axis',(0.,1.,0.));
#10250=DIRECTION('ref_axis',(1.,0.,0.));
#10251=DIRECTION('',(0.,-1.,0.));
#10252=DIRECTION('center_axis',(0.,1.,0.));
#10253=DIRECTION('ref_axis',(1.,0.,0.));
#10254=DIRECTION('center_axis',(0.,1.,0.));
#10255=DIRECTION('ref_axis',(1.,0.,0.));
#10256=DIRECTION('center_axis',(0.,1.,0.));
#10257=DIRECTION('ref_axis',(1.,0.,0.));
#10258=DIRECTION('axis',(0.,0.,1.));
#10259=DIRECTION('refdir',(1.,0.,0.));
#10260=DIRECTION('center_axis',(0.,1.,0.));
#10261=DIRECTION('ref_axis',(1.,0.,0.));
#10262=DIRECTION('center_axis',(0.,-1.,0.));
#10263=DIRECTION('ref_axis',(1.,0.,0.));
#10264=DIRECTION('',(0.,-1.,0.));
#10265=DIRECTION('center_axis',(0.,-1.,0.));
#10266=DIRECTION('ref_axis',(1.,0.,0.));
#10267=DIRECTION('center_axis',(0.,1.,0.));
#10268=DIRECTION('ref_axis',(1.,0.,0.));
#10269=DIRECTION('center_axis',(0.,1.,0.));
#10270=DIRECTION('ref_axis',(1.,0.,0.));
#10271=DIRECTION('',(0.,-1.,0.));
#10272=DIRECTION('center_axis',(0.,1.,0.));
#10273=DIRECTION('ref_axis',(1.,0.,0.));
#10274=DIRECTION('center_axis',(0.,1.,0.));
#10275=DIRECTION('ref_axis',(1.,0.,0.));
#10276=DIRECTION('center_axis',(0.,1.,0.));
#10277=DIRECTION('ref_axis',(1.,0.,0.));
#10278=DIRECTION('axis',(0.,0.,1.));
#10279=DIRECTION('refdir',(1.,0.,0.));
#10280=DIRECTION('center_axis',(0.,1.,0.));
#10281=DIRECTION('ref_axis',(1.,0.,0.));
#10282=DIRECTION('center_axis',(0.,1.,0.));
#10283=DIRECTION('ref_axis',(1.,0.,0.));
#10284=DIRECTION('',(0.,1.,0.));
#10285=DIRECTION('center_axis',(0.,-1.,0.));
#10286=DIRECTION('ref_axis',(1.,0.,0.));
#10287=DIRECTION('center_axis',(0.,1.,0.));
#10288=DIRECTION('ref_axis',(1.,0.,0.));
#10289=DIRECTION('center_axis',(0.,1.,0.));
#10290=DIRECTION('ref_axis',(1.,0.,0.));
#10291=DIRECTION('',(0.,1.,0.));
#10292=DIRECTION('center_axis',(0.,-1.,0.));
#10293=DIRECTION('ref_axis',(1.,0.,0.));
#10294=DIRECTION('center_axis',(0.,1.,0.));
#10295=DIRECTION('ref_axis',(1.,0.,0.));
#10296=DIRECTION('center_axis',(0.,1.,0.));
#10297=DIRECTION('ref_axis',(1.,0.,0.));
#10298=DIRECTION('',(0.,1.,0.));
#10299=DIRECTION('center_axis',(0.,-1.,0.));
#10300=DIRECTION('ref_axis',(1.,0.,0.));
#10301=DIRECTION('center_axis',(0.,1.,0.));
#10302=DIRECTION('ref_axis',(1.,0.,0.));
#10303=DIRECTION('center_axis',(0.,1.,0.));
#10304=DIRECTION('ref_axis',(1.,0.,0.));
#10305=DIRECTION('',(0.,1.,0.));
#10306=DIRECTION('center_axis',(0.,-1.,0.));
#10307=DIRECTION('ref_axis',(1.,0.,0.));
#10308=DIRECTION('center_axis',(0.,1.,0.));
#10309=DIRECTION('ref_axis',(1.,0.,0.));
#10310=DIRECTION('center_axis',(0.,-1.,0.));
#10311=DIRECTION('ref_axis',(1.,0.,0.));
#10312=DIRECTION('',(0.,-1.,0.));
#10313=DIRECTION('center_axis',(0.,-1.,0.));
#10314=DIRECTION('ref_axis',(1.,0.,0.));
#10315=DIRECTION('center_axis',(0.,1.,0.));
#10316=DIRECTION('ref_axis',(1.,0.,0.));
#10317=DIRECTION('center_axis',(0.,1.,0.));
#10318=DIRECTION('ref_axis',(1.,0.,0.));
#10319=DIRECTION('',(0.,-1.,0.));
#10320=DIRECTION('center_axis',(0.,1.,0.));
#10321=DIRECTION('ref_axis',(1.,0.,0.));
#10322=DIRECTION('center_axis',(0.,1.,0.));
#10323=DIRECTION('ref_axis',(1.,0.,0.));
#10324=DIRECTION('center_axis',(0.,1.,0.));
#10325=DIRECTION('ref_axis',(1.,0.,0.));
#10326=DIRECTION('axis',(0.,0.,1.));
#10327=DIRECTION('refdir',(1.,0.,0.));
#10328=DIRECTION('center_axis',(0.,1.,0.));
#10329=DIRECTION('ref_axis',(1.,0.,0.));
#10330=DIRECTION('center_axis',(0.,1.,0.));
#10331=DIRECTION('ref_axis',(1.,0.,0.));
#10332=DIRECTION('',(0.,1.,0.));
#10333=DIRECTION('center_axis',(0.,-1.,0.));
#10334=DIRECTION('ref_axis',(1.,0.,0.));
#10335=DIRECTION('center_axis',(0.,1.,0.));
#10336=DIRECTION('ref_axis',(1.,0.,0.));
#10337=DIRECTION('center_axis',(0.,1.,0.));
#10338=DIRECTION('ref_axis',(1.,0.,0.));
#10339=DIRECTION('',(0.,1.,0.));
#10340=DIRECTION('center_axis',(0.,-1.,0.));
#10341=DIRECTION('ref_axis',(1.,0.,0.));
#10342=DIRECTION('center_axis',(0.,1.,0.));
#10343=DIRECTION('ref_axis',(1.,0.,0.));
#10344=DIRECTION('center_axis',(0.,1.,0.));
#10345=DIRECTION('ref_axis',(1.,0.,0.));
#10346=DIRECTION('',(0.,1.,0.));
#10347=DIRECTION('center_axis',(0.,-1.,0.));
#10348=DIRECTION('ref_axis',(1.,0.,0.));
#10349=DIRECTION('center_axis',(0.,1.,0.));
#10350=DIRECTION('ref_axis',(1.,0.,0.));
#10351=DIRECTION('center_axis',(0.,1.,0.));
#10352=DIRECTION('ref_axis',(1.,0.,0.));
#10353=DIRECTION('',(0.,1.,0.));
#10354=DIRECTION('center_axis',(0.,-1.,0.));
#10355=DIRECTION('ref_axis',(1.,0.,0.));
#10356=DIRECTION('center_axis',(0.,1.,0.));
#10357=DIRECTION('ref_axis',(1.,0.,0.));
#10358=DIRECTION('center_axis',(0.,-1.,0.));
#10359=DIRECTION('ref_axis',(1.,0.,0.));
#10360=DIRECTION('',(0.,-1.,0.));
#10361=DIRECTION('center_axis',(0.,-1.,0.));
#10362=DIRECTION('ref_axis',(1.,0.,0.));
#10363=DIRECTION('center_axis',(0.,1.,0.));
#10364=DIRECTION('ref_axis',(1.,0.,0.));
#10365=DIRECTION('center_axis',(0.,1.,0.));
#10366=DIRECTION('ref_axis',(1.,0.,0.));
#10367=DIRECTION('',(0.,-1.,0.));
#10368=DIRECTION('center_axis',(0.,1.,0.));
#10369=DIRECTION('ref_axis',(1.,0.,0.));
#10370=DIRECTION('center_axis',(0.,1.,0.));
#10371=DIRECTION('ref_axis',(1.,0.,0.));
#10372=DIRECTION('center_axis',(0.,1.,0.));
#10373=DIRECTION('ref_axis',(1.,0.,0.));
#10374=DIRECTION('axis',(0.,0.,1.));
#10375=DIRECTION('refdir',(1.,0.,0.));
#10376=DIRECTION('axis',(0.,0.,1.));
#10377=DIRECTION('refdir',(1.,0.,0.));
#10378=DIRECTION('center_axis',(0.,-1.,0.));
#10379=DIRECTION('ref_axis',(0.,0.,-1.));
#10380=DIRECTION('center_axis',(0.,-1.,0.));
#10381=DIRECTION('ref_axis',(1.,0.,0.));
#10382=DIRECTION('center_axis',(0.,-1.,0.));
#10383=DIRECTION('ref_axis',(1.,0.,0.));
#10384=DIRECTION('center_axis',(1.,0.,1.22464679914735E-16));
#10385=DIRECTION('ref_axis',(-1.22464679914735E-16,0.,1.));
#10386=DIRECTION('center_axis',(0.,1.,0.));
#10387=DIRECTION('ref_axis',(1.,0.,0.));
#10388=DIRECTION('center_axis',(0.,1.,0.));
#10389=DIRECTION('ref_axis',(1.,0.,0.));
#10390=DIRECTION('center_axis',(0.,-1.,0.));
#10391=DIRECTION('ref_axis',(1.,0.,0.));
#10392=DIRECTION('',(0.,1.,0.));
#10393=DIRECTION('center_axis',(0.,-1.,0.));
#10394=DIRECTION('ref_axis',(1.,0.,0.));
#10395=DIRECTION('center_axis',(0.,-1.,0.));
#10396=DIRECTION('ref_axis',(1.,0.,0.));
#10397=DIRECTION('center_axis',(0.,-1.,0.));
#10398=DIRECTION('ref_axis',(1.,0.,0.));
#10399=DIRECTION('',(0.,1.,0.));
#10400=DIRECTION('center_axis',(0.,-1.,0.));
#10401=DIRECTION('ref_axis',(1.,0.,0.));
#10402=DIRECTION('center_axis',(0.,1.,0.));
#10403=DIRECTION('ref_axis',(1.,0.,0.));
#10404=DIRECTION('',(-0.707106781186547,0.707106781186548,-8.65956056235493E-17));
#10405=DIRECTION('center_axis',(0.,-1.,0.));
#10406=DIRECTION('ref_axis',(1.,0.,0.));
#10407=DIRECTION('center_axis',(0.,1.,0.));
#10408=DIRECTION('ref_axis',(0.,0.,1.));
#10409=DIRECTION('center_axis',(0.,-1.,0.));
#10410=DIRECTION('ref_axis',(1.,0.,0.));
#10411=DIRECTION('center_axis',(0.,-1.,0.));
#10412=DIRECTION('ref_axis',(1.,0.,0.));
#10413=DIRECTION('',(0.,1.,0.));
#10414=DIRECTION('center_axis',(0.,-1.,0.));
#10415=DIRECTION('ref_axis',(0.,0.,-1.));
#10416=DIRECTION('center_axis',(0.,-1.,0.));
#10417=DIRECTION('ref_axis',(1.,0.,0.));
#10418=DIRECTION('center_axis',(0.,-1.,0.));
#10419=DIRECTION('ref_axis',(1.,0.,0.));
#10420=DIRECTION('',(0.707106781186547,0.707106781186548,8.65956056235493E-17));
#10421=DIRECTION('axis',(0.,0.,1.));
#10422=DIRECTION('refdir',(1.,0.,0.));
#10423=DIRECTION('center_axis',(0.,-1.,0.));
#10424=DIRECTION('ref_axis',(0.,0.,-1.));
#10425=DIRECTION('center_axis',(0.,-1.,0.));
#10426=DIRECTION('ref_axis',(1.,0.,0.));
#10427=DIRECTION('center_axis',(0.,-1.,0.));
#10428=DIRECTION('ref_axis',(1.,0.,0.));
#10429=DIRECTION('center_axis',(1.,0.,1.22464679914735E-16));
#10430=DIRECTION('ref_axis',(-1.22464679914735E-16,0.,1.));
#10431=DIRECTION('center_axis',(0.,1.,0.));
#10432=DIRECTION('ref_axis',(1.,0.,0.));
#10433=DIRECTION('center_axis',(0.,1.,0.));
#10434=DIRECTION('ref_axis',(1.,0.,0.));
#10435=DIRECTION('center_axis',(0.,-1.,0.));
#10436=DIRECTION('ref_axis',(1.,0.,0.));
#10437=DIRECTION('center_axis',(0.,-1.,0.));
#10438=DIRECTION('ref_axis',(1.,0.,0.));
#10439=DIRECTION('',(0.,1.,0.));
#10440=DIRECTION('center_axis',(0.,1.,0.));
#10441=DIRECTION('ref_axis',(0.,0.,1.));
#10442=DIRECTION('center_axis',(0.,-1.,0.));
#10443=DIRECTION('ref_axis',(1.,0.,0.));
#10444=DIRECTION('center_axis',(0.,-1.,0.));
#10445=DIRECTION('ref_axis',(1.,0.,0.));
#10446=DIRECTION('center_axis',(0.,-1.,0.));
#10447=DIRECTION('ref_axis',(1.,0.,0.));
#10448=DIRECTION('center_axis',(0.,-1.,0.));
#10449=DIRECTION('ref_axis',(1.,0.,0.));
#10450=DIRECTION('',(0.707106781186548,0.707106781186547,8.65956056235494E-17));
#10451=DIRECTION('center_axis',(0.,-1.,0.));
#10452=DIRECTION('ref_axis',(1.,0.,0.));
#10453=DIRECTION('center_axis',(0.,-1.,0.));
#10454=DIRECTION('ref_axis',(1.,0.,0.));
#10455=DIRECTION('',(0.,1.,0.));
#10456=DIRECTION('center_axis',(0.,1.,0.));
#10457=DIRECTION('ref_axis',(1.,0.,0.));
#10458=DIRECTION('center_axis',(0.,-1.,0.));
#10459=DIRECTION('ref_axis',(1.,0.,0.));
#10460=DIRECTION('',(-0.707106781186548,0.707106781186547,-8.65956056235494E-17));
#10461=DIRECTION('center_axis',(0.,-1.,0.));
#10462=DIRECTION('ref_axis',(0.,0.,-1.));
#10463=DIRECTION('center_axis',(0.,-1.,0.));
#10464=DIRECTION('ref_axis',(1.,0.,0.));
#10465=DIRECTION('',(0.,1.,0.));
#10466=DIRECTION('axis',(0.,0.,1.));
#10467=DIRECTION('refdir',(1.,0.,0.));
#10468=DIRECTION('center_axis',(0.,0.,1.));
#10469=DIRECTION('ref_axis',(1.,0.,0.));
#10470=DIRECTION('center_axis',(1.22464679914735E-16,-1.,0.));
#10471=DIRECTION('ref_axis',(-1.,-1.22464679914735E-16,0.));
#10472=DIRECTION('center_axis',(0.707106781186548,0.,0.707106781186548));
#10473=DIRECTION('ref_axis',(0.707106781186548,0.,-0.707106781186548));
#10474=DIRECTION('center_axis',(8.65956056235494E-17,-1.,-8.65956056235493E-17));
#10475=DIRECTION('ref_axis',(-0.707106781186547,-1.22464679914735E-16,0.707106781186547));
#10476=DIRECTION('center_axis',(1.,0.,0.));
#10477=DIRECTION('ref_axis',(6.12323399573676E-17,0.,-1.));
#10478=DIRECTION('center_axis',(7.49879891330929E-33,-1.,-1.22464679914735E-16));
#10479=DIRECTION('ref_axis',(-6.12323399573676E-17,-1.22464679914735E-16,
1.));
#10480=DIRECTION('center_axis',(0.707106781186548,0.,-0.707106781186548));
#10481=DIRECTION('ref_axis',(-0.707106781186548,0.,-0.707106781186548));
#10482=DIRECTION('center_axis',(-8.65956056235493E-17,-1.,-8.65956056235494E-17));
#10483=DIRECTION('ref_axis',(0.707106781186547,-1.22464679914735E-16,0.707106781186547));
#10484=DIRECTION('center_axis',(0.,0.,-1.));
#10485=DIRECTION('ref_axis',(-1.,0.,-1.22464679914735E-16));
#10486=DIRECTION('center_axis',(-1.22464679914735E-16,-1.,-1.49975978266186E-32));
#10487=DIRECTION('ref_axis',(1.,-1.22464679914735E-16,1.22464679914735E-16));
#10488=DIRECTION('center_axis',(-0.707106781186547,0.,-0.707106781186548));
#10489=DIRECTION('ref_axis',(-0.707106781186548,0.,0.707106781186547));
#10490=DIRECTION('center_axis',(-8.65956056235493E-17,-1.,8.65956056235493E-17));
#10491=DIRECTION('ref_axis',(0.707106781186548,-1.22464679914735E-16,-0.707106781186547));
#10492=DIRECTION('center_axis',(-1.,0.,0.));
#10493=DIRECTION('ref_axis',(-1.83697019872103E-16,0.,1.));
#10494=DIRECTION('center_axis',(-2.24963967399279E-32,-1.,1.22464679914735E-16));
#10495=DIRECTION('ref_axis',(1.83697019872103E-16,-1.22464679914735E-16,
-1.));
#10496=DIRECTION('center_axis',(-0.707106781186548,0.,0.707106781186548));
#10497=DIRECTION('ref_axis',(0.707106781186547,0.,0.707106781186548));
#10498=DIRECTION('center_axis',(8.65956056235493E-17,-1.,8.65956056235493E-17));
#10499=DIRECTION('ref_axis',(-0.707106781186547,-1.22464679914735E-16,-0.707106781186548));
#10500=DIRECTION('axis',(0.,0.,1.));
#10501=DIRECTION('refdir',(1.,0.,0.));
#10502=DIRECTION('center_axis',(0.,0.,1.));
#10503=DIRECTION('ref_axis',(1.,0.,0.));
#10504=DIRECTION('center_axis',(0.,-1.,0.));
#10505=DIRECTION('ref_axis',(0.,0.,-1.));
#10506=DIRECTION('center_axis',(0.,-1.,0.));
#10507=DIRECTION('ref_axis',(0.,0.,-1.));
#10508=DIRECTION('center_axis',(0.,1.,0.));
#10509=DIRECTION('ref_axis',(1.,0.,0.));
#10510=DIRECTION('center_axis',(0.,1.,0.));
#10511=DIRECTION('ref_axis',(1.,0.,0.));
#10512=DIRECTION('center_axis',(0.,1.,0.));
#10513=DIRECTION('ref_axis',(1.,0.,0.));
#10514=DIRECTION('center_axis',(0.,1.,0.));
#10515=DIRECTION('ref_axis',(1.,0.,0.));
#10516=DIRECTION('',(0.,-1.,0.));
#10517=DIRECTION('center_axis',(0.,-1.,0.));
#10518=DIRECTION('ref_axis',(1.,0.,0.));
#10519=DIRECTION('center_axis',(0.,1.,0.));
#10520=DIRECTION('ref_axis',(1.,0.,0.));
#10521=DIRECTION('center_axis',(0.,1.,0.));
#10522=DIRECTION('ref_axis',(1.,0.,0.));
#10523=DIRECTION('center_axis',(0.,1.,0.));
#10524=DIRECTION('ref_axis',(1.,0.,0.));
#10525=DIRECTION('center_axis',(0.,1.,0.));
#10526=DIRECTION('ref_axis',(1.,0.,0.));
#10527=DIRECTION('center_axis',(0.,1.,0.));
#10528=DIRECTION('ref_axis',(1.,0.,0.));
#10529=DIRECTION('center_axis',(0.,1.,0.));
#10530=DIRECTION('ref_axis',(1.,0.,0.));
#10531=DIRECTION('center_axis',(0.,-1.,0.));
#10532=DIRECTION('ref_axis',(1.,0.,0.));
#10533=DIRECTION('center_axis',(0.,-1.,0.));
#10534=DIRECTION('ref_axis',(0.,0.,-1.));
#10535=DIRECTION('center_axis',(6.12323399573677E-17,0.,1.));
#10536=DIRECTION('ref_axis',(1.,0.,0.));
#10537=DIRECTION('center_axis',(0.,-1.,0.));
#10538=DIRECTION('ref_axis',(0.,0.,-1.));
#10539=DIRECTION('center_axis',(0.,1.,0.));
#10540=DIRECTION('ref_axis',(1.,0.,0.));
#10541=DIRECTION('center_axis',(0.,-1.,0.));
#10542=DIRECTION('ref_axis',(1.,0.,0.));
#10543=DIRECTION('center_axis',(0.,-1.,0.));
#10544=DIRECTION('ref_axis',(0.,0.,-1.));
#10545=DIRECTION('center_axis',(0.,0.,1.));
#10546=DIRECTION('ref_axis',(1.,0.,0.));
#10547=DIRECTION('center_axis',(0.,-1.,0.));
#10548=DIRECTION('ref_axis',(0.,0.,-1.));
#10549=DIRECTION('center_axis',(0.,1.,0.));
#10550=DIRECTION('ref_axis',(1.,0.,0.));
#10551=DIRECTION('center_axis',(0.,-1.,0.));
#10552=DIRECTION('ref_axis',(1.,0.,0.));
#10553=DIRECTION('center_axis',(0.,-1.,0.));
#10554=DIRECTION('ref_axis',(0.,0.,-1.));
#10555=DIRECTION('center_axis',(0.,0.,1.));
#10556=DIRECTION('ref_axis',(1.,0.,0.));
#10557=DIRECTION('center_axis',(0.,-1.,0.));
#10558=DIRECTION('ref_axis',(0.,0.,-1.));
#10559=DIRECTION('center_axis',(0.,1.,0.));
#10560=DIRECTION('ref_axis',(1.,0.,0.));
#10561=DIRECTION('center_axis',(0.,-1.,0.));
#10562=DIRECTION('ref_axis',(1.,0.,0.));
#10563=DIRECTION('center_axis',(0.,-1.,0.));
#10564=DIRECTION('ref_axis',(0.,0.,-1.));
#10565=DIRECTION('center_axis',(0.,0.,1.));
#10566=DIRECTION('ref_axis',(1.,0.,0.));
#10567=DIRECTION('center_axis',(0.,-1.,0.));
#10568=DIRECTION('ref_axis',(0.,0.,-1.));
#10569=DIRECTION('center_axis',(0.,1.,0.));
#10570=DIRECTION('ref_axis',(1.,0.,0.));
#10571=DIRECTION('center_axis',(0.,-1.,0.));
#10572=DIRECTION('ref_axis',(1.,0.,0.));
#10573=DIRECTION('center_axis',(0.,-1.,0.));
#10574=DIRECTION('ref_axis',(0.,0.,-1.));
#10575=DIRECTION('center_axis',(6.12323399573676E-17,0.,1.));
#10576=DIRECTION('ref_axis',(1.,0.,0.));
#10577=DIRECTION('center_axis',(0.,-1.,0.));
#10578=DIRECTION('ref_axis',(0.,0.,-1.));
#10579=DIRECTION('center_axis',(0.,1.,0.));
#10580=DIRECTION('ref_axis',(1.,0.,0.));
#10581=DIRECTION('center_axis',(0.,-1.,0.));
#10582=DIRECTION('ref_axis',(1.,0.,0.));
#10583=DIRECTION('center_axis',(0.,-1.,0.));
#10584=DIRECTION('ref_axis',(0.,0.,-1.));
#10585=DIRECTION('center_axis',(0.,0.,1.));
#10586=DIRECTION('ref_axis',(1.,0.,0.));
#10587=DIRECTION('center_axis',(0.,-1.,0.));
#10588=DIRECTION('ref_axis',(0.,0.,-1.));
#10589=DIRECTION('center_axis',(0.,1.,0.));
#10590=DIRECTION('ref_axis',(1.,0.,0.));
#10591=DIRECTION('center_axis',(0.,1.,0.));
#10592=DIRECTION('ref_axis',(1.,0.,0.));
#10593=DIRECTION('',(0.,1.,0.));
#10594=DIRECTION('center_axis',(0.,-1.,0.));
#10595=DIRECTION('ref_axis',(1.,0.,0.));
#10596=DIRECTION('center_axis',(0.,-1.,0.));
#10597=DIRECTION('ref_axis',(1.,0.,0.));
#10598=DIRECTION('center_axis',(0.,1.,0.));
#10599=DIRECTION('ref_axis',(1.,0.,0.));
#10600=DIRECTION('center_axis',(0.,-1.,0.));
#10601=DIRECTION('ref_axis',(0.,0.,-1.));
#10602=DIRECTION('center_axis',(0.,0.,1.));
#10603=DIRECTION('ref_axis',(1.,0.,0.));
#10604=DIRECTION('center_axis',(0.,-1.,0.));
#10605=DIRECTION('ref_axis',(0.,0.,-1.));
#10606=DIRECTION('center_axis',(0.,-1.,0.));
#10607=DIRECTION('ref_axis',(-1.,0.,0.));
#10608=DIRECTION('center_axis',(0.,1.,0.));
#10609=DIRECTION('ref_axis',(1.,0.,0.));
#10610=DIRECTION('axis',(0.,0.,1.));
#10611=DIRECTION('refdir',(1.,0.,0.));
#10612=DIRECTION('center_axis',(0.,1.,0.));
#10613=DIRECTION('ref_axis',(0.,0.,1.));
#10614=DIRECTION('center_axis',(0.,-1.,0.));
#10615=DIRECTION('ref_axis',(1.,0.,0.));
#10616=DIRECTION('center_axis',(0.,-1.,0.));
#10617=DIRECTION('ref_axis',(1.,0.,0.));
#10618=DIRECTION('center_axis',(0.,-1.,0.));
#10619=DIRECTION('ref_axis',(1.,0.,0.));
#10620=DIRECTION('center_axis',(0.,-1.,0.));
#10621=DIRECTION('ref_axis',(1.,0.,0.));
#10622=DIRECTION('',(0.,1.,0.));
#10623=DIRECTION('center_axis',(0.,-1.,0.));
#10624=DIRECTION('ref_axis',(0.,0.,-1.));
#10625=DIRECTION('center_axis',(0.,-1.,0.));
#10626=DIRECTION('ref_axis',(1.,0.,0.));
#10627=DIRECTION('center_axis',(0.,-1.,0.));
#10628=DIRECTION('ref_axis',(1.,0.,0.));
#10629=DIRECTION('',(0.,1.,0.));
#10630=DIRECTION('center_axis',(0.,1.,0.));
#10631=DIRECTION('ref_axis',(0.,0.,1.));
#10632=DIRECTION('center_axis',(0.,-1.,0.));
#10633=DIRECTION('ref_axis',(1.,0.,0.));
#10634=DIRECTION('center_axis',(0.,-1.,0.));
#10635=DIRECTION('ref_axis',(1.,0.,0.));
#10636=DIRECTION('center_axis',(0.,-1.,0.));
#10637=DIRECTION('ref_axis',(1.,0.,0.));
#10638=DIRECTION('center_axis',(0.,-1.,0.));
#10639=DIRECTION('ref_axis',(1.,0.,0.));
#10640=DIRECTION('',(0.,1.,0.));
#10641=DIRECTION('center_axis',(0.,-1.,0.));
#10642=DIRECTION('ref_axis',(0.,0.,-1.));
#10643=DIRECTION('center_axis',(0.,-1.,0.));
#10644=DIRECTION('ref_axis',(1.,0.,0.));
#10645=DIRECTION('center_axis',(0.,-1.,0.));
#10646=DIRECTION('ref_axis',(1.,0.,0.));
#10647=DIRECTION('',(0.,1.,0.));
#10648=DIRECTION('',(0.,0.,1.));
#10649=DIRECTION('',(1.,0.,0.));
#10650=DIRECTION('',(0.,0.,1.));
#10651=DIRECTION('',(1.,0.,0.));
#10652=DIRECTION('',(0.,0.,1.));
#10653=DIRECTION('',(1.,0.,0.));
#10654=DIRECTION('',(0.,0.,1.));
#10655=DIRECTION('',(1.,0.,0.));
#10656=DIRECTION('',(0.,0.,1.));
#10657=DIRECTION('',(1.,0.,0.));
#10658=DIRECTION('axis',(0.,0.,1.));
#10659=DIRECTION('refdir',(1.,0.,0.));
#10660=DIRECTION('center_axis',(0.866025403784439,0.,-0.5));
#10661=DIRECTION('ref_axis',(0.5,0.,0.866025403784439));
#10662=DIRECTION('',(-0.5,0.,-0.866025403784439));
#10663=DIRECTION('',(0.,-1.,0.));
#10664=DIRECTION('',(0.5,0.,0.866025403784439));
#10665=DIRECTION('',(0.,-1.,0.));
#10666=DIRECTION('center_axis',(1.60246890531964E-16,0.,-1.));
#10667=DIRECTION('ref_axis',(1.,0.,1.60246890531964E-16));
#10668=DIRECTION('',(-1.,0.,-1.60246890531964E-16));
#10669=DIRECTION('',(0.,-1.,0.));
#10670=DIRECTION('',(1.,0.,1.60246890531964E-16));
#10671=DIRECTION('center_axis',(-0.866025403784439,0.,-0.5));
#10672=DIRECTION('ref_axis',(0.5,0.,-0.866025403784439));
#10673=DIRECTION('',(-0.5,0.,0.866025403784439));
#10674=DIRECTION('',(0.,-1.,0.));
#10675=DIRECTION('',(0.5,0.,-0.866025403784439));
#10676=DIRECTION('center_axis',(-0.866025403784439,0.,0.5));
#10677=DIRECTION('ref_axis',(-0.5,0.,-0.866025403784439));
#10678=DIRECTION('',(0.5,0.,0.866025403784439));
#10679=DIRECTION('',(0.,-1.,0.));
#10680=DIRECTION('',(-0.5,0.,-0.866025403784439));
#10681=DIRECTION('center_axis',(-1.60246890531964E-16,0.,1.));
#10682=DIRECTION('ref_axis',(-1.,0.,-1.60246890531964E-16));
#10683=DIRECTION('',(1.,0.,1.60246890531964E-16));
#10684=DIRECTION('',(0.,-1.,0.));
#10685=DIRECTION('',(-1.,0.,-1.60246890531964E-16));
#10686=DIRECTION('center_axis',(0.866025403784439,0.,0.5));
#10687=DIRECTION('ref_axis',(-0.5,0.,0.866025403784439));
#10688=DIRECTION('',(0.5,0.,-0.866025403784439));
#10689=DIRECTION('',(-0.5,0.,0.866025403784439));
#10690=DIRECTION('center_axis',(0.,1.,0.));
#10691=DIRECTION('ref_axis',(1.,0.,0.));
#10692=DIRECTION('center_axis',(0.,-1.,0.));
#10693=DIRECTION('ref_axis',(0.,0.,-1.));
#10694=DIRECTION('center_axis',(0.,1.,0.));
#10695=DIRECTION('ref_axis',(1.,0.,0.));
#10696=DIRECTION('center_axis',(0.,1.,0.));
#10697=DIRECTION('ref_axis',(1.,0.,0.));
#10698=DIRECTION('center_axis',(0.,1.,0.));
#10699=DIRECTION('ref_axis',(0.,0.,1.));
#10700=DIRECTION('center_axis',(0.,-1.,0.));
#10701=DIRECTION('ref_axis',(1.,0.,0.));
#10702=DIRECTION('center_axis',(0.,-1.,0.));
#10703=DIRECTION('ref_axis',(1.,0.,0.));
#10704=DIRECTION('center_axis',(0.,-1.,0.));
#10705=DIRECTION('ref_axis',(1.,0.,0.));
#10706=DIRECTION('',(0.707106781186547,0.707106781186548,8.65956056235493E-17));
#10707=DIRECTION('center_axis',(0.,-1.,0.));
#10708=DIRECTION('ref_axis',(1.,0.,0.));
#10709=DIRECTION('center_axis',(0.,-1.,0.));
#10710=DIRECTION('ref_axis',(1.,0.,0.));
#10711=DIRECTION('',(0.,1.,0.));
#10712=DIRECTION('center_axis',(0.,1.,0.));
#10713=DIRECTION('ref_axis',(1.,0.,0.));
#10714=DIRECTION('center_axis',(0.,-1.,0.));
#10715=DIRECTION('ref_axis',(1.,0.,0.));
#10716=DIRECTION('',(-0.707106781186547,0.707106781186548,-8.65956056235493E-17));
#10717=DIRECTION('center_axis',(0.,-1.,0.));
#10718=DIRECTION('ref_axis',(0.,0.,-1.));
#10719=DIRECTION('center_axis',(0.,-1.,0.));
#10720=DIRECTION('ref_axis',(1.,0.,0.));
#10721=DIRECTION('center_axis',(0.,1.,0.));
#10722=DIRECTION('ref_axis',(1.,0.,0.));
#10723=DIRECTION('center_axis',(0.,1.,0.));
#10724=DIRECTION('ref_axis',(1.,0.,0.));
#10725=DIRECTION('',(-0.447213595499958,0.894427190999916,-5.47678698264203E-17));
#10726=DIRECTION('center_axis',(0.,-1.,0.));
#10727=DIRECTION('ref_axis',(1.,0.,0.));
#10728=DIRECTION('',(0.,1.,0.));
#10729=DIRECTION('',(0.,0.,1.));
#10730=DIRECTION('',(1.,0.,0.));
#10731=DIRECTION('',(0.,0.,1.));
#10732=DIRECTION('',(1.,0.,0.));
#10733=DIRECTION('',(0.,0.,1.));
#10734=DIRECTION('',(1.,0.,0.));
#10735=DIRECTION('',(0.,0.,1.));
#10736=DIRECTION('',(1.,0.,0.));
#10737=DIRECTION('',(0.,0.,1.));
#10738=DIRECTION('',(1.,0.,0.));
#10739=DIRECTION('',(0.,0.,1.));
#10740=DIRECTION('',(1.,0.,0.));
#10741=DIRECTION('',(0.,0.,1.));
#10742=DIRECTION('',(1.,0.,0.));
#10743=DIRECTION('',(0.,0.,1.));
#10744=DIRECTION('',(1.,0.,0.));
#10745=DIRECTION('',(0.,0.,1.));
#10746=DIRECTION('',(1.,0.,0.));
#10747=DIRECTION('',(0.,0.,1.));
#10748=DIRECTION('',(1.,0.,0.));
#10749=DIRECTION('',(0.,0.,1.));
#10750=DIRECTION('',(-1.,1.22464679914735E-16,0.));
#10751=DIRECTION('',(0.,0.,1.));
#10752=DIRECTION('',(-1.,1.22464679914735E-16,0.));
#10753=DIRECTION('',(0.,0.,1.));
#10754=DIRECTION('',(-1.,1.22464679914735E-16,0.));
#10755=DIRECTION('',(0.,0.,1.));
#10756=DIRECTION('',(-1.,1.22464679914735E-16,0.));
#10757=DIRECTION('',(0.,0.,1.));
#10758=DIRECTION('',(1.,0.,0.));
#10759=DIRECTION('',(0.,0.,1.));
#10760=DIRECTION('',(1.,0.,0.));
#10761=DIRECTION('',(0.,0.,1.));
#10762=DIRECTION('',(1.,0.,0.));
#10763=DIRECTION('',(0.,0.,1.));
#10764=DIRECTION('',(1.,0.,0.));
#10765=DIRECTION('',(0.,0.,1.));
#10766=DIRECTION('',(1.,0.,0.));
#10767=DIRECTION('',(0.,0.,1.));
#10768=DIRECTION('',(1.,0.,0.));
#10769=DIRECTION('',(0.,0.,1.));
#10770=DIRECTION('',(-1.,1.22464679914735E-16,0.));
#10771=DIRECTION('',(0.,0.,1.));
#10772=DIRECTION('',(-1.,1.22464679914735E-16,0.));
#10773=DIRECTION('',(0.,0.,1.));
#10774=DIRECTION('',(-1.,1.22464679914735E-16,0.));
#10775=DIRECTION('',(0.,0.,1.));
#10776=DIRECTION('',(-1.,1.22464679914735E-16,0.));
#10777=DIRECTION('',(0.,0.,1.));
#10778=DIRECTION('',(1.,0.,0.));
#10779=DIRECTION('',(0.,0.,1.));
#10780=DIRECTION('',(1.,0.,0.));
#10781=DIRECTION('',(0.,0.,1.));
#10782=DIRECTION('',(1.,0.,0.));
#10783=DIRECTION('',(0.,0.,1.));
#10784=DIRECTION('',(1.,0.,0.));
#10785=DIRECTION('',(0.,0.,1.));
#10786=DIRECTION('',(1.,0.,0.));
#10787=DIRECTION('',(0.,0.,1.));
#10788=DIRECTION('',(1.,0.,0.));
#10789=DIRECTION('',(0.,0.,1.));
#10790=DIRECTION('',(1.,0.,0.));
#10791=DIRECTION('',(0.,0.,1.));
#10792=DIRECTION('',(1.,0.,0.));
#10793=DIRECTION('',(0.,0.,1.));
#10794=DIRECTION('',(1.,0.,0.));
#10795=DIRECTION('',(0.,0.,1.));
#10796=DIRECTION('',(1.,0.,0.));
#10797=DIRECTION('',(0.,0.,1.));
#10798=DIRECTION('',(1.,0.,0.));
#10799=DIRECTION('',(0.,0.,1.));
#10800=DIRECTION('',(1.,0.,0.));
#10801=DIRECTION('',(0.,0.,1.));
#10802=DIRECTION('',(1.,0.,0.));
#10803=DIRECTION('',(0.,0.,1.));
#10804=DIRECTION('',(-1.,1.22464679914735E-16,0.));
#10805=DIRECTION('',(0.,0.,1.));
#10806=DIRECTION('',(-1.,1.22464679914735E-16,0.));
#10807=DIRECTION('',(0.,0.,1.));
#10808=DIRECTION('',(-1.,1.22464679914735E-16,0.));
#10809=DIRECTION('',(0.,0.,1.));
#10810=DIRECTION('',(-1.,1.22464679914735E-16,0.));
#10811=DIRECTION('',(0.,0.,1.));
#10812=DIRECTION('',(1.,0.,0.));
#10813=DIRECTION('',(0.,0.,1.));
#10814=DIRECTION('',(1.,0.,0.));
#10815=DIRECTION('',(0.,0.,1.));
#10816=DIRECTION('',(1.,0.,0.));
#10817=DIRECTION('',(0.,0.,1.));
#10818=DIRECTION('',(1.,0.,0.));
#10819=DIRECTION('',(0.,0.,1.));
#10820=DIRECTION('',(1.,0.,0.));
#10821=DIRECTION('',(0.,0.,1.));
#10822=DIRECTION('',(1.,0.,0.));
#10823=DIRECTION('',(0.,0.,1.));
#10824=DIRECTION('',(-1.,1.22464679914735E-16,0.));
#10825=DIRECTION('',(0.,0.,1.));
#10826=DIRECTION('',(-1.,1.22464679914735E-16,0.));
#10827=DIRECTION('',(0.,0.,1.));
#10828=DIRECTION('',(-1.,1.22464679914735E-16,0.));
#10829=DIRECTION('',(0.,0.,1.));
#10830=DIRECTION('',(-1.,1.22464679914735E-16,0.));
#10831=DIRECTION('',(0.,0.,1.));
#10832=DIRECTION('',(1.,0.,0.));
#10833=DIRECTION('',(0.,0.,1.));
#10834=DIRECTION('',(1.,0.,0.));
#10835=DIRECTION('',(0.,0.,1.));
#10836=DIRECTION('',(1.,0.,0.));
#10837=DIRECTION('',(0.,0.,1.));
#10838=DIRECTION('',(1.,0.,0.));
#10839=DIRECTION('axis',(0.,0.,1.));
#10840=DIRECTION('refdir',(1.,0.,0.));
#10841=DIRECTION('axis',(0.,0.,1.));
#10842=DIRECTION('refdir',(1.,0.,0.));
#10843=DIRECTION('center_axis',(0.,1.,0.));
#10844=DIRECTION('ref_axis',(1.,0.,0.));
#10845=DIRECTION('center_axis',(0.,1.,0.));
#10846=DIRECTION('ref_axis',(1.,0.,0.));
#10847=DIRECTION('',(0.,1.,0.));
#10848=DIRECTION('center_axis',(0.,-1.,0.));
#10849=DIRECTION('ref_axis',(1.,0.,0.));
#10850=DIRECTION('center_axis',(0.,1.,0.));
#10851=DIRECTION('ref_axis',(1.,0.,0.));
#10852=DIRECTION('center_axis',(0.,1.,0.));
#10853=DIRECTION('ref_axis',(1.,0.,0.));
#10854=DIRECTION('',(0.,1.,0.));
#10855=DIRECTION('center_axis',(0.,-1.,0.));
#10856=DIRECTION('ref_axis',(1.,0.,0.));
#10857=DIRECTION('center_axis',(0.,1.,0.));
#10858=DIRECTION('ref_axis',(1.,0.,0.));
#10859=DIRECTION('center_axis',(0.,1.,0.));
#10860=DIRECTION('ref_axis',(1.,0.,0.));
#10861=DIRECTION('',(0.,1.,0.));
#10862=DIRECTION('center_axis',(0.,-1.,0.));
#10863=DIRECTION('ref_axis',(1.,0.,0.));
#10864=DIRECTION('center_axis',(0.,1.,0.));
#10865=DIRECTION('ref_axis',(1.,0.,0.));
#10866=DIRECTION('center_axis',(0.,1.,0.));
#10867=DIRECTION('ref_axis',(1.,0.,0.));
#10868=DIRECTION('',(0.,1.,0.));
#10869=DIRECTION('center_axis',(0.,-1.,0.));
#10870=DIRECTION('ref_axis',(1.,0.,0.));
#10871=DIRECTION('center_axis',(0.,1.,0.));
#10872=DIRECTION('ref_axis',(1.,0.,0.));
#10873=DIRECTION('center_axis',(0.,1.,0.));
#10874=DIRECTION('ref_axis',(1.,0.,0.));
#10875=DIRECTION('',(0.,1.,0.));
#10876=DIRECTION('center_axis',(0.,-1.,0.));
#10877=DIRECTION('ref_axis',(1.,0.,0.));
#10878=DIRECTION('center_axis',(0.,1.,0.));
#10879=DIRECTION('ref_axis',(1.,0.,0.));
#10880=DIRECTION('center_axis',(0.,1.,0.));
#10881=DIRECTION('ref_axis',(1.,0.,0.));
#10882=DIRECTION('',(0.,1.,0.));
#10883=DIRECTION('center_axis',(0.,-1.,0.));
#10884=DIRECTION('ref_axis',(1.,0.,0.));
#10885=DIRECTION('center_axis',(0.,1.,0.));
#10886=DIRECTION('ref_axis',(1.,0.,0.));
#10887=DIRECTION('center_axis',(0.,1.,0.));
#10888=DIRECTION('ref_axis',(1.,0.,0.));
#10889=DIRECTION('',(0.,1.,0.));
#10890=DIRECTION('center_axis',(0.,-1.,0.));
#10891=DIRECTION('ref_axis',(1.,0.,0.));
#10892=DIRECTION('center_axis',(0.,1.,0.));
#10893=DIRECTION('ref_axis',(1.,0.,0.));
#10894=DIRECTION('center_axis',(0.,1.,0.));
#10895=DIRECTION('ref_axis',(1.,0.,0.));
#10896=DIRECTION('',(0.,1.,0.));
#10897=DIRECTION('center_axis',(0.,-1.,0.));
#10898=DIRECTION('ref_axis',(1.,0.,0.));
#10899=DIRECTION('center_axis',(0.,0.,1.));
#10900=DIRECTION('ref_axis',(1.,0.,0.));
#10901=DIRECTION('center_axis',(0.,0.,1.));
#10902=DIRECTION('ref_axis',(1.,0.,0.));
#10903=DIRECTION('',(0.,0.,1.));
#10904=DIRECTION('center_axis',(0.,0.,-1.));
#10905=DIRECTION('ref_axis',(1.,0.,0.));
#10906=DIRECTION('center_axis',(0.,0.,1.));
#10907=DIRECTION('ref_axis',(1.,0.,0.));
#10908=DIRECTION('center_axis',(0.,0.,1.));
#10909=DIRECTION('ref_axis',(1.,0.,0.));
#10910=DIRECTION('',(0.,0.,1.));
#10911=DIRECTION('center_axis',(0.,0.,-1.));
#10912=DIRECTION('ref_axis',(1.,0.,0.));
#10913=DIRECTION('center_axis',(0.,0.,1.));
#10914=DIRECTION('ref_axis',(1.,0.,0.));
#10915=DIRECTION('center_axis',(0.,0.,1.));
#10916=DIRECTION('ref_axis',(1.,0.,0.));
#10917=DIRECTION('',(0.,0.,1.));
#10918=DIRECTION('center_axis',(0.,0.,-1.));
#10919=DIRECTION('ref_axis',(1.,0.,0.));
#10920=DIRECTION('center_axis',(0.,0.,1.));
#10921=DIRECTION('ref_axis',(1.,0.,0.));
#10922=DIRECTION('center_axis',(0.,0.,1.));
#10923=DIRECTION('ref_axis',(1.,0.,0.));
#10924=DIRECTION('',(0.,0.,1.));
#10925=DIRECTION('center_axis',(0.,0.,-1.));
#10926=DIRECTION('ref_axis',(1.,0.,0.));
#10927=DIRECTION('center_axis',(0.,1.,0.));
#10928=DIRECTION('ref_axis',(-1.,0.,0.));
#10929=DIRECTION('',(-1.,0.,0.));
#10930=DIRECTION('',(0.,0.,1.));
#10931=DIRECTION('',(-1.,0.,0.));
#10932=DIRECTION('',(0.,0.,1.));
#10933=DIRECTION('center_axis',(1.,0.,0.));
#10934=DIRECTION('ref_axis',(0.,1.,0.));
#10935=DIRECTION('',(0.,1.,0.));
#10936=DIRECTION('',(0.,1.,0.));
#10937=DIRECTION('',(0.,0.,1.));
#10938=DIRECTION('center_axis',(0.,0.,1.));
#10939=DIRECTION('ref_axis',(1.,0.,0.));
#10940=DIRECTION('',(0.,-1.,0.));
#10941=DIRECTION('',(1.,0.,0.));
#10942=DIRECTION('center_axis',(0.,0.,1.));
#10943=DIRECTION('ref_axis',(1.,0.,0.));
#10944=DIRECTION('',(-1.,0.,0.));
#10945=DIRECTION('',(0.,-1.,0.));
#10946=DIRECTION('',(1.,0.,0.));
#10947=DIRECTION('',(0.,1.,0.));
#10948=DIRECTION('center_axis',(0.,1.,0.));
#10949=DIRECTION('ref_axis',(-1.,0.,0.));
#10950=DIRECTION('',(-1.,0.,0.));
#10951=DIRECTION('',(0.,0.,1.));
#10952=DIRECTION('',(0.,0.,1.));
#10953=DIRECTION('center_axis',(1.,0.,0.));
#10954=DIRECTION('ref_axis',(0.,1.,0.));
#10955=DIRECTION('',(0.,1.,0.));
#10956=DIRECTION('',(0.,0.,1.));
#10957=DIRECTION('center_axis',(0.,-1.,0.));
#10958=DIRECTION('ref_axis',(1.,0.,0.));
#10959=DIRECTION('',(1.,0.,0.));
#10960=DIRECTION('',(0.,0.,1.));
#10961=DIRECTION('center_axis',(-1.,0.,0.));
#10962=DIRECTION('ref_axis',(0.,-1.,0.));
#10963=DIRECTION('',(0.,-1.,0.));
#10964=DIRECTION('center_axis',(0.,0.,1.));
#10965=DIRECTION('ref_axis',(1.,0.,0.));
#10966=DIRECTION('axis',(0.,0.,1.));
#10967=DIRECTION('refdir',(1.,0.,0.));
#10968=DIRECTION('center_axis',(0.,1.,0.));
#10969=DIRECTION('ref_axis',(1.,0.,0.));
#10970=DIRECTION('center_axis',(0.,1.,0.));
#10971=DIRECTION('ref_axis',(1.,0.,0.));
#10972=DIRECTION('',(0.,1.,0.));
#10973=DIRECTION('center_axis',(0.,1.,0.));
#10974=DIRECTION('ref_axis',(1.,0.,0.));
#10975=DIRECTION('center_axis',(0.,1.,0.));
#10976=DIRECTION('ref_axis',(1.,0.,0.));
#10977=DIRECTION('center_axis',(0.,1.,0.));
#10978=DIRECTION('ref_axis',(1.,0.,0.));
#10979=DIRECTION('center_axis',(0.,1.,0.));
#10980=DIRECTION('ref_axis',(1.,0.,0.));
#10981=DIRECTION('',(0.,1.,0.));
#10982=DIRECTION('center_axis',(0.,-1.,0.));
#10983=DIRECTION('ref_axis',(1.,0.,0.));
#10984=DIRECTION('center_axis',(0.,1.,0.));
#10985=DIRECTION('ref_axis',(1.,0.,0.));
#10986=DIRECTION('center_axis',(0.,1.,0.));
#10987=DIRECTION('ref_axis',(1.,0.,0.));
#10988=DIRECTION('',(0.,1.,0.));
#10989=DIRECTION('center_axis',(0.,-1.,0.));
#10990=DIRECTION('ref_axis',(1.,0.,0.));
#10991=DIRECTION('center_axis',(0.,1.,0.));
#10992=DIRECTION('ref_axis',(1.,0.,0.));
#10993=DIRECTION('center_axis',(0.,1.,0.));
#10994=DIRECTION('ref_axis',(1.,0.,0.));
#10995=DIRECTION('',(0.,1.,0.));
#10996=DIRECTION('center_axis',(0.,-1.,0.));
#10997=DIRECTION('ref_axis',(1.,0.,0.));
#10998=DIRECTION('center_axis',(0.,1.,0.));
#10999=DIRECTION('ref_axis',(1.,0.,0.));
#11000=DIRECTION('center_axis',(0.,1.,0.));
#11001=DIRECTION('ref_axis',(1.,0.,0.));
#11002=DIRECTION('center_axis',(0.,1.,0.));
#11003=DIRECTION('ref_axis',(1.,0.,0.));
#11004=DIRECTION('center_axis',(0.,1.,0.));
#11005=DIRECTION('ref_axis',(1.,0.,0.));
#11006=DIRECTION('center_axis',(0.,1.,0.));
#11007=DIRECTION('ref_axis',(1.,0.,0.));
#11008=DIRECTION('center_axis',(0.,-1.,0.));
#11009=DIRECTION('ref_axis',(1.,0.,0.));
#11010=DIRECTION('center_axis',(0.,1.,0.));
#11011=DIRECTION('ref_axis',(1.,0.,0.));
#11012=DIRECTION('',(0.,-1.,0.));
#11013=DIRECTION('center_axis',(0.,1.,0.));
#11014=DIRECTION('ref_axis',(1.,0.,0.));
#11015=DIRECTION('',(0.,-1.,0.));
#11016=DIRECTION('center_axis',(0.,1.,0.));
#11017=DIRECTION('ref_axis',(1.,0.,0.));
#11018=DIRECTION('center_axis',(0.,1.,0.));
#11019=DIRECTION('ref_axis',(1.,0.,0.));
#11020=DIRECTION('center_axis',(0.,1.,0.));
#11021=DIRECTION('ref_axis',(1.,0.,0.));
#11022=DIRECTION('',(0.,-1.,0.));
#11023=DIRECTION('center_axis',(0.,1.,0.));
#11024=DIRECTION('ref_axis',(1.,0.,0.));
#11025=DIRECTION('center_axis',(0.,1.,0.));
#11026=DIRECTION('ref_axis',(1.,0.,0.));
#11027=DIRECTION('axis',(0.,0.,1.));
#11028=DIRECTION('refdir',(1.,0.,0.));
#11029=DIRECTION('center_axis',(0.,1.,0.));
#11030=DIRECTION('ref_axis',(1.,0.,0.));
#11031=DIRECTION('center_axis',(0.,-1.,0.));
#11032=DIRECTION('ref_axis',(1.,0.,0.));
#11033=DIRECTION('',(0.,-1.,0.));
#11034=DIRECTION('center_axis',(0.,-1.,0.));
#11035=DIRECTION('ref_axis',(1.,0.,0.));
#11036=DIRECTION('center_axis',(0.,1.,0.));
#11037=DIRECTION('ref_axis',(1.,0.,0.));
#11038=DIRECTION('center_axis',(0.,1.,0.));
#11039=DIRECTION('ref_axis',(1.,0.,0.));
#11040=DIRECTION('',(0.,-1.,0.));
#11041=DIRECTION('center_axis',(0.,1.,0.));
#11042=DIRECTION('ref_axis',(1.,0.,0.));
#11043=DIRECTION('center_axis',(0.,1.,0.));
#11044=DIRECTION('ref_axis',(1.,0.,0.));
#11045=DIRECTION('center_axis',(0.,1.,0.));
#11046=DIRECTION('ref_axis',(1.,0.,0.));
#11047=DIRECTION('axis',(0.,0.,1.));
#11048=DIRECTION('refdir',(1.,0.,0.));
#11049=DIRECTION('center_axis',(0.,1.,0.));
#11050=DIRECTION('ref_axis',(1.,0.,0.));
#11051=DIRECTION('center_axis',(0.,-1.,0.));
#11052=DIRECTION('ref_axis',(1.,0.,0.));
#11053=DIRECTION('',(0.,-1.,0.));
#11054=DIRECTION('center_axis',(0.,-1.,0.));
#11055=DIRECTION('ref_axis',(1.,0.,0.));
#11056=DIRECTION('center_axis',(0.,1.,0.));
#11057=DIRECTION('ref_axis',(1.,0.,0.));
#11058=DIRECTION('center_axis',(0.,1.,0.));
#11059=DIRECTION('ref_axis',(1.,0.,0.));
#11060=DIRECTION('',(0.,-1.,0.));
#11061=DIRECTION('center_axis',(0.,1.,0.));
#11062=DIRECTION('ref_axis',(1.,0.,0.));
#11063=DIRECTION('center_axis',(0.,1.,0.));
#11064=DIRECTION('ref_axis',(1.,0.,0.));
#11065=DIRECTION('center_axis',(0.,1.,0.));
#11066=DIRECTION('ref_axis',(1.,0.,0.));
#11067=DIRECTION('axis',(0.,0.,1.));
#11068=DIRECTION('refdir',(1.,0.,0.));
#11069=DIRECTION('center_axis',(0.,1.,0.));
#11070=DIRECTION('ref_axis',(1.,0.,0.));
#11071=DIRECTION('center_axis',(0.,-1.,0.));
#11072=DIRECTION('ref_axis',(1.,0.,0.));
#11073=DIRECTION('',(0.,-1.,0.));
#11074=DIRECTION('center_axis',(0.,-1.,0.));
#11075=DIRECTION('ref_axis',(1.,0.,0.));
#11076=DIRECTION('center_axis',(0.,1.,0.));
#11077=DIRECTION('ref_axis',(1.,0.,0.));
#11078=DIRECTION('center_axis',(0.,1.,0.));
#11079=DIRECTION('ref_axis',(1.,0.,0.));
#11080=DIRECTION('',(0.,-1.,0.));
#11081=DIRECTION('center_axis',(0.,1.,0.));
#11082=DIRECTION('ref_axis',(1.,0.,0.));
#11083=DIRECTION('center_axis',(0.,1.,0.));
#11084=DIRECTION('ref_axis',(1.,0.,0.));
#11085=DIRECTION('center_axis',(0.,1.,0.));
#11086=DIRECTION('ref_axis',(1.,0.,0.));
#11087=DIRECTION('axis',(0.,0.,1.));
#11088=DIRECTION('refdir',(1.,0.,0.));
#11089=DIRECTION('center_axis',(0.,1.,0.));
#11090=DIRECTION('ref_axis',(1.,0.,0.));
#11091=DIRECTION('center_axis',(0.,-1.,0.));
#11092=DIRECTION('ref_axis',(1.,0.,0.));
#11093=DIRECTION('',(0.,-1.,0.));
#11094=DIRECTION('center_axis',(0.,-1.,0.));
#11095=DIRECTION('ref_axis',(1.,0.,0.));
#11096=DIRECTION('center_axis',(0.,1.,0.));
#11097=DIRECTION('ref_axis',(1.,0.,0.));
#11098=DIRECTION('center_axis',(0.,1.,0.));
#11099=DIRECTION('ref_axis',(1.,0.,0.));
#11100=DIRECTION('',(0.,-1.,0.));
#11101=DIRECTION('center_axis',(0.,1.,0.));
#11102=DIRECTION('ref_axis',(1.,0.,0.));
#11103=DIRECTION('center_axis',(0.,1.,0.));
#11104=DIRECTION('ref_axis',(1.,0.,0.));
#11105=DIRECTION('center_axis',(0.,1.,0.));
#11106=DIRECTION('ref_axis',(1.,0.,0.));
#11107=DIRECTION('axis',(0.,0.,1.));
#11108=DIRECTION('refdir',(1.,0.,0.));
#11109=DIRECTION('center_axis',(0.,1.,0.));
#11110=DIRECTION('ref_axis',(1.,0.,0.));
#11111=DIRECTION('center_axis',(0.,1.,0.));
#11112=DIRECTION('ref_axis',(1.,0.,0.));
#11113=DIRECTION('',(0.,1.,0.));
#11114=DIRECTION('center_axis',(0.,1.,0.));
#11115=DIRECTION('ref_axis',(1.,0.,0.));
#11116=DIRECTION('center_axis',(0.,1.,0.));
#11117=DIRECTION('ref_axis',(1.,0.,0.));
#11118=DIRECTION('center_axis',(0.,1.,0.));
#11119=DIRECTION('ref_axis',(1.,0.,0.));
#11120=DIRECTION('center_axis',(0.,1.,0.));
#11121=DIRECTION('ref_axis',(1.,0.,0.));
#11122=DIRECTION('',(0.,1.,0.));
#11123=DIRECTION('center_axis',(0.,-1.,0.));
#11124=DIRECTION('ref_axis',(1.,0.,0.));
#11125=DIRECTION('center_axis',(0.,1.,0.));
#11126=DIRECTION('ref_axis',(1.,0.,0.));
#11127=DIRECTION('center_axis',(0.,1.,0.));
#11128=DIRECTION('ref_axis',(1.,0.,0.));
#11129=DIRECTION('',(0.,1.,0.));
#11130=DIRECTION('center_axis',(0.,-1.,0.));
#11131=DIRECTION('ref_axis',(1.,0.,0.));
#11132=DIRECTION('center_axis',(0.,1.,0.));
#11133=DIRECTION('ref_axis',(1.,0.,0.));
#11134=DIRECTION('center_axis',(0.,1.,0.));
#11135=DIRECTION('ref_axis',(1.,0.,0.));
#11136=DIRECTION('',(0.,1.,0.));
#11137=DIRECTION('center_axis',(0.,-1.,0.));
#11138=DIRECTION('ref_axis',(1.,0.,0.));
#11139=DIRECTION('center_axis',(0.,1.,0.));
#11140=DIRECTION('ref_axis',(1.,0.,0.));
#11141=DIRECTION('center_axis',(0.,1.,0.));
#11142=DIRECTION('ref_axis',(1.,0.,0.));
#11143=DIRECTION('center_axis',(0.,1.,0.));
#11144=DIRECTION('ref_axis',(1.,0.,0.));
#11145=DIRECTION('center_axis',(0.,1.,0.));
#11146=DIRECTION('ref_axis',(1.,0.,0.));
#11147=DIRECTION('center_axis',(0.,1.,0.));
#11148=DIRECTION('ref_axis',(1.,0.,0.));
#11149=DIRECTION('center_axis',(0.,-1.,0.));
#11150=DIRECTION('ref_axis',(1.,0.,0.));
#11151=DIRECTION('center_axis',(0.,1.,0.));
#11152=DIRECTION('ref_axis',(1.,0.,0.));
#11153=DIRECTION('',(0.,-1.,0.));
#11154=DIRECTION('center_axis',(0.,1.,0.));
#11155=DIRECTION('ref_axis',(1.,0.,0.));
#11156=DIRECTION('',(0.,-1.,0.));
#11157=DIRECTION('center_axis',(0.,1.,0.));
#11158=DIRECTION('ref_axis',(1.,0.,0.));
#11159=DIRECTION('center_axis',(0.,1.,0.));
#11160=DIRECTION('ref_axis',(1.,0.,0.));
#11161=DIRECTION('center_axis',(0.,1.,0.));
#11162=DIRECTION('ref_axis',(1.,0.,0.));
#11163=DIRECTION('',(0.,-1.,0.));
#11164=DIRECTION('center_axis',(0.,1.,0.));
#11165=DIRECTION('ref_axis',(1.,0.,0.));
#11166=DIRECTION('center_axis',(0.,1.,0.));
#11167=DIRECTION('ref_axis',(1.,0.,0.));
#11168=DIRECTION('axis',(0.,0.,1.));
#11169=DIRECTION('refdir',(1.,0.,0.));
#11170=DIRECTION('center_axis',(0.,1.,0.));
#11171=DIRECTION('ref_axis',(1.,0.,0.));
#11172=DIRECTION('center_axis',(0.,-1.,0.));
#11173=DIRECTION('ref_axis',(1.,0.,0.));
#11174=DIRECTION('',(0.,-1.,0.));
#11175=DIRECTION('center_axis',(0.,-1.,0.));
#11176=DIRECTION('ref_axis',(1.,0.,0.));
#11177=DIRECTION('center_axis',(0.,1.,0.));
#11178=DIRECTION('ref_axis',(1.,0.,0.));
#11179=DIRECTION('center_axis',(0.,1.,0.));
#11180=DIRECTION('ref_axis',(1.,0.,0.));
#11181=DIRECTION('',(0.,-1.,0.));
#11182=DIRECTION('center_axis',(0.,1.,0.));
#11183=DIRECTION('ref_axis',(1.,0.,0.));
#11184=DIRECTION('center_axis',(0.,1.,0.));
#11185=DIRECTION('ref_axis',(1.,0.,0.));
#11186=DIRECTION('center_axis',(0.,1.,0.));
#11187=DIRECTION('ref_axis',(1.,0.,0.));
#11188=DIRECTION('axis',(0.,0.,1.));
#11189=DIRECTION('refdir',(1.,0.,0.));
#11190=DIRECTION('center_axis',(0.,1.,0.));
#11191=DIRECTION('ref_axis',(1.,0.,0.));
#11192=DIRECTION('center_axis',(0.,-1.,0.));
#11193=DIRECTION('ref_axis',(1.,0.,0.));
#11194=DIRECTION('',(0.,-1.,0.));
#11195=DIRECTION('center_axis',(0.,-1.,0.));
#11196=DIRECTION('ref_axis',(1.,0.,0.));
#11197=DIRECTION('center_axis',(0.,1.,0.));
#11198=DIRECTION('ref_axis',(1.,0.,0.));
#11199=DIRECTION('center_axis',(0.,1.,0.));
#11200=DIRECTION('ref_axis',(1.,0.,0.));
#11201=DIRECTION('',(0.,-1.,0.));
#11202=DIRECTION('center_axis',(0.,1.,0.));
#11203=DIRECTION('ref_axis',(1.,0.,0.));
#11204=DIRECTION('center_axis',(0.,1.,0.));
#11205=DIRECTION('ref_axis',(1.,0.,0.));
#11206=DIRECTION('center_axis',(0.,1.,0.));
#11207=DIRECTION('ref_axis',(1.,0.,0.));
#11208=DIRECTION('axis',(0.,0.,1.));
#11209=DIRECTION('refdir',(1.,0.,0.));
#11210=DIRECTION('center_axis',(0.,1.,0.));
#11211=DIRECTION('ref_axis',(1.,0.,0.));
#11212=DIRECTION('center_axis',(0.,-1.,0.));
#11213=DIRECTION('ref_axis',(1.,0.,0.));
#11214=DIRECTION('',(0.,-1.,0.));
#11215=DIRECTION('center_axis',(0.,-1.,0.));
#11216=DIRECTION('ref_axis',(1.,0.,0.));
#11217=DIRECTION('center_axis',(0.,1.,0.));
#11218=DIRECTION('ref_axis',(1.,0.,0.));
#11219=DIRECTION('center_axis',(0.,1.,0.));
#11220=DIRECTION('ref_axis',(1.,0.,0.));
#11221=DIRECTION('',(0.,-1.,0.));
#11222=DIRECTION('center_axis',(0.,1.,0.));
#11223=DIRECTION('ref_axis',(1.,0.,0.));
#11224=DIRECTION('center_axis',(0.,1.,0.));
#11225=DIRECTION('ref_axis',(1.,0.,0.));
#11226=DIRECTION('center_axis',(0.,1.,0.));
#11227=DIRECTION('ref_axis',(1.,0.,0.));
#11228=DIRECTION('axis',(0.,0.,1.));
#11229=DIRECTION('refdir',(1.,0.,0.));
#11230=DIRECTION('center_axis',(0.,1.,0.));
#11231=DIRECTION('ref_axis',(1.,0.,0.));
#11232=DIRECTION('center_axis',(0.,-1.,0.));
#11233=DIRECTION('ref_axis',(1.,0.,0.));
#11234=DIRECTION('',(0.,-1.,0.));
#11235=DIRECTION('center_axis',(0.,-1.,0.));
#11236=DIRECTION('ref_axis',(1.,0.,0.));
#11237=DIRECTION('center_axis',(0.,1.,0.));
#11238=DIRECTION('ref_axis',(1.,0.,0.));
#11239=DIRECTION('center_axis',(0.,1.,0.));
#11240=DIRECTION('ref_axis',(1.,0.,0.));
#11241=DIRECTION('',(0.,-1.,0.));
#11242=DIRECTION('center_axis',(0.,1.,0.));
#11243=DIRECTION('ref_axis',(1.,0.,0.));
#11244=DIRECTION('center_axis',(0.,1.,0.));
#11245=DIRECTION('ref_axis',(1.,0.,0.));
#11246=DIRECTION('center_axis',(0.,1.,0.));
#11247=DIRECTION('ref_axis',(1.,0.,0.));
#11248=DIRECTION('axis',(0.,0.,1.));
#11249=DIRECTION('refdir',(1.,0.,0.));
#11250=DIRECTION('center_axis',(0.,1.,0.));
#11251=DIRECTION('ref_axis',(0.,0.,1.));
#11252=DIRECTION('center_axis',(0.,-1.,0.));
#11253=DIRECTION('ref_axis',(1.,0.,0.));
#11254=DIRECTION('center_axis',(0.,-1.,0.));
#11255=DIRECTION('ref_axis',(1.,0.,0.));
#11256=DIRECTION('center_axis',(0.,-1.,0.));
#11257=DIRECTION('ref_axis',(1.,0.,0.));
#11258=DIRECTION('',(0.707106781186547,0.707106781186548,8.65956056235493E-17));
#11259=DIRECTION('center_axis',(0.,-1.,0.));
#11260=DIRECTION('ref_axis',(1.,0.,0.));
#11261=DIRECTION('center_axis',(0.,-1.,0.));
#11262=DIRECTION('ref_axis',(1.,0.,0.));
#11263=DIRECTION('',(0.,1.,0.));
#11264=DIRECTION('center_axis',(0.,1.,0.));
#11265=DIRECTION('ref_axis',(1.,0.,0.));
#11266=DIRECTION('center_axis',(0.,-1.,0.));
#11267=DIRECTION('ref_axis',(1.,0.,0.));
#11268=DIRECTION('',(-0.707106781186547,0.707106781186548,-8.65956056235493E-17));
#11269=DIRECTION('center_axis',(0.,-1.,0.));
#11270=DIRECTION('ref_axis',(0.,0.,-1.));
#11271=DIRECTION('center_axis',(0.,-1.,0.));
#11272=DIRECTION('ref_axis',(1.,0.,0.));
#11273=DIRECTION('center_axis',(0.,1.,0.));
#11274=DIRECTION('ref_axis',(1.,0.,0.));
#11275=DIRECTION('center_axis',(0.,1.,0.));
#11276=DIRECTION('ref_axis',(1.,0.,0.));
#11277=DIRECTION('',(-0.447213595499958,0.894427190999916,-5.47678698264203E-17));
#11278=DIRECTION('center_axis',(0.,-1.,0.));
#11279=DIRECTION('ref_axis',(1.,0.,0.));
#11280=DIRECTION('center_axis',(0.,1.,0.));
#11281=DIRECTION('ref_axis',(1.,0.,0.));
#11282=DIRECTION('',(0.,1.,0.));
#11283=DIRECTION('center_axis',(0.,1.,0.));
#11284=DIRECTION('ref_axis',(1.,0.,0.));
#11285=DIRECTION('center_axis',(0.,-1.,0.));
#11286=DIRECTION('ref_axis',(1.,0.,0.));
#11287=DIRECTION('',(-0.707106781186547,0.707106781186548,-8.65956056235493E-17));
#11288=DIRECTION('center_axis',(0.,-1.,0.));
#11289=DIRECTION('ref_axis',(0.,0.,-1.));
#11290=DIRECTION('center_axis',(0.866025403784439,0.,-0.5));
#11291=DIRECTION('ref_axis',(0.5,0.,0.866025403784439));
#11292=DIRECTION('',(-0.5,0.,-0.866025403784439));
#11293=DIRECTION('',(0.,-1.,0.));
#11294=DIRECTION('',(0.5,0.,0.866025403784439));
#11295=DIRECTION('',(0.,-1.,0.));
#11296=DIRECTION('center_axis',(1.60246890531964E-16,0.,-1.));
#11297=DIRECTION('ref_axis',(1.,0.,1.60246890531964E-16));
#11298=DIRECTION('',(-1.,0.,-1.60246890531964E-16));
#11299=DIRECTION('',(0.,-1.,0.));
#11300=DIRECTION('',(1.,0.,1.60246890531964E-16));
#11301=DIRECTION('center_axis',(-0.866025403784439,0.,-0.5));
#11302=DIRECTION('ref_axis',(0.5,0.,-0.866025403784439));
#11303=DIRECTION('',(-0.5,0.,0.866025403784439));
#11304=DIRECTION('',(0.,-1.,0.));
#11305=DIRECTION('',(0.5,0.,-0.866025403784439));
#11306=DIRECTION('center_axis',(-0.866025403784439,0.,0.5));
#11307=DIRECTION('ref_axis',(-0.5,0.,-0.866025403784439));
#11308=DIRECTION('',(0.5,0.,0.866025403784439));
#11309=DIRECTION('',(0.,-1.,0.));
#11310=DIRECTION('',(-0.5,0.,-0.866025403784439));
#11311=DIRECTION('center_axis',(-1.60246890531964E-16,0.,1.));
#11312=DIRECTION('ref_axis',(-1.,0.,-1.60246890531964E-16));
#11313=DIRECTION('',(1.,0.,1.60246890531964E-16));
#11314=DIRECTION('',(0.,-1.,0.));
#11315=DIRECTION('',(-1.,0.,-1.60246890531964E-16));
#11316=DIRECTION('center_axis',(0.866025403784439,0.,0.5));
#11317=DIRECTION('ref_axis',(-0.5,0.,0.866025403784439));
#11318=DIRECTION('',(0.5,0.,-0.866025403784439));
#11319=DIRECTION('',(-0.5,0.,0.866025403784439));
#11320=DIRECTION('center_axis',(0.,1.,0.));
#11321=DIRECTION('ref_axis',(1.,0.,0.));
#11322=DIRECTION('center_axis',(0.,-1.,0.));
#11323=DIRECTION('ref_axis',(0.,0.,-1.));
#11324=DIRECTION('',(0.,0.,1.));
#11325=DIRECTION('',(1.,0.,0.));
#11326=DIRECTION('',(0.,0.,1.));
#11327=DIRECTION('',(1.,0.,0.));
#11328=DIRECTION('',(0.,0.,1.));
#11329=DIRECTION('',(1.,0.,0.));
#11330=DIRECTION('',(0.,0.,1.));
#11331=DIRECTION('',(1.,0.,0.));
#11332=DIRECTION('',(0.,0.,1.));
#11333=DIRECTION('',(1.,0.,0.));
#11334=DIRECTION('',(0.,0.,1.));
#11335=DIRECTION('',(1.,0.,0.));
#11336=DIRECTION('',(0.,0.,1.));
#11337=DIRECTION('',(1.,0.,0.));
#11338=DIRECTION('',(0.,0.,1.));
#11339=DIRECTION('',(1.,0.,0.));
#11340=DIRECTION('',(0.,0.,1.));
#11341=DIRECTION('',(1.,0.,0.));
#11342=DIRECTION('',(0.,0.,1.));
#11343=DIRECTION('',(1.,0.,0.));
#11344=DIRECTION('',(0.,0.,1.));
#11345=DIRECTION('',(1.,0.,0.));
#11346=DIRECTION('',(0.,0.,1.));
#11347=DIRECTION('',(1.,0.,0.));
#11348=DIRECTION('',(0.,0.,1.));
#11349=DIRECTION('',(1.,0.,0.));
#11350=DIRECTION('',(0.,0.,1.));
#11351=DIRECTION('',(1.,0.,0.));
#11352=DIRECTION('',(0.,0.,1.));
#11353=DIRECTION('',(1.,0.,0.));
#11354=DIRECTION('',(0.,0.,1.));
#11355=DIRECTION('',(1.,0.,0.));
#11356=DIRECTION('',(0.,-1.,2.22044604925031E-16));
#11357=DIRECTION('',(1.,0.,0.));
#11358=DIRECTION('',(0.,-1.,2.22044604925031E-16));
#11359=DIRECTION('',(1.,0.,0.));
#11360=DIRECTION('',(0.,-1.,2.22044604925031E-16));
#11361=DIRECTION('',(1.,0.,0.));
#11362=DIRECTION('',(0.,-1.,2.22044604925031E-16));
#11363=DIRECTION('',(1.,0.,0.));
#11364=DIRECTION('',(0.,0.,1.));
#11365=DIRECTION('',(-1.,1.22464679914735E-16,0.));
#11366=DIRECTION('',(0.,0.,1.));
#11367=DIRECTION('',(-1.,1.22464679914735E-16,0.));
#11368=DIRECTION('',(0.,0.,1.));
#11369=DIRECTION('',(-1.,1.22464679914735E-16,0.));
#11370=DIRECTION('',(0.,0.,1.));
#11371=DIRECTION('',(-1.,1.22464679914735E-16,0.));
#11372=DIRECTION('',(0.,0.,1.));
#11373=DIRECTION('',(-1.,1.22464679914735E-16,0.));
#11374=DIRECTION('',(0.,0.,1.));
#11375=DIRECTION('',(-1.,1.22464679914735E-16,0.));
#11376=DIRECTION('',(0.,0.,1.));
#11377=DIRECTION('',(-1.,1.22464679914735E-16,0.));
#11378=DIRECTION('',(0.,0.,1.));
#11379=DIRECTION('',(-1.,1.22464679914735E-16,0.));
#11380=DIRECTION('',(0.,0.,1.));
#11381=DIRECTION('',(2.22044604925031E-16,1.,0.));
#11382=DIRECTION('',(0.,0.,1.));
#11383=DIRECTION('',(1.,0.,0.));
#11384=DIRECTION('',(0.,0.,1.));
#11385=DIRECTION('',(1.,0.,0.));
#11386=DIRECTION('',(0.,0.,1.));
#11387=DIRECTION('',(1.,0.,0.));
#11388=DIRECTION('',(0.,0.,1.));
#11389=DIRECTION('',(1.,0.,0.));
#11390=DIRECTION('',(0.,0.,1.));
#11391=DIRECTION('',(1.,0.,0.));
#11392=DIRECTION('',(0.,0.,1.));
#11393=DIRECTION('',(1.,0.,0.));
#11394=DIRECTION('',(0.,0.,1.));
#11395=DIRECTION('',(1.,0.,0.));
#11396=DIRECTION('',(0.,0.,1.));
#11397=DIRECTION('',(1.,0.,0.));
#11398=DIRECTION('',(0.,0.,1.));
#11399=DIRECTION('',(1.,0.,0.));
#11400=DIRECTION('',(0.,0.,1.));
#11401=DIRECTION('',(1.,0.,0.));
#11402=DIRECTION('',(0.,0.,1.));
#11403=DIRECTION('',(1.,0.,0.));
#11404=DIRECTION('',(0.,0.,1.));
#11405=DIRECTION('',(-1.,1.22464679914735E-16,0.));
#11406=DIRECTION('',(0.,0.,1.));
#11407=DIRECTION('',(-1.,1.22464679914735E-16,0.));
#11408=DIRECTION('',(0.,0.,1.));
#11409=DIRECTION('',(-1.,1.22464679914735E-16,0.));
#11410=DIRECTION('',(0.,0.,1.));
#11411=DIRECTION('',(-1.,1.22464679914735E-16,0.));
#11412=DIRECTION('',(0.,0.,1.));
#11413=DIRECTION('',(-1.,1.22464679914735E-16,0.));
#11414=DIRECTION('',(0.,0.,1.));
#11415=DIRECTION('',(-1.,1.22464679914735E-16,0.));
#11416=DIRECTION('',(0.,0.,1.));
#11417=DIRECTION('',(-1.,1.22464679914735E-16,0.));
#11418=DIRECTION('',(0.,0.,1.));
#11419=DIRECTION('',(-1.,1.22464679914735E-16,0.));
#11420=DIRECTION('',(0.,0.,1.));
#11421=DIRECTION('',(1.,0.,0.));
#11422=DIRECTION('',(0.,0.,1.));
#11423=DIRECTION('',(1.,0.,0.));
#11424=DIRECTION('',(0.,0.,1.));
#11425=DIRECTION('',(1.,0.,0.));
#11426=DIRECTION('',(0.,0.,1.));
#11427=DIRECTION('',(1.,0.,0.));
#11428=CARTESIAN_POINT('',(0.,0.,0.));
#11429=CARTESIAN_POINT('',(0.,0.,0.));
#11430=CARTESIAN_POINT('',(0.,0.,0.));
#11431=CARTESIAN_POINT('Origin',(3.2,3.5,-0.1));
#11432=CARTESIAN_POINT('',(2.99,3.5,0.));
#11433=CARTESIAN_POINT('Origin',(3.2,3.5,0.));
#11434=CARTESIAN_POINT('',(2.99,3.5,1.));
#11435=CARTESIAN_POINT('',(2.99,3.5,-0.1));
#11436=CARTESIAN_POINT('Origin',(3.2,3.5,1.));
#11437=CARTESIAN_POINT('Origin',(-3.2,5.5,-0.1));
#11438=CARTESIAN_POINT('',(-3.41,5.5,0.));
#11439=CARTESIAN_POINT('Origin',(-3.2,5.5,0.));
#11440=CARTESIAN_POINT('',(-3.41,5.5,1.));
#11441=CARTESIAN_POINT('',(-3.41,5.5,-0.1));
#11442=CARTESIAN_POINT('Origin',(-3.2,5.5,1.));
#11443=CARTESIAN_POINT('Origin',(-3.2,3.5,-0.1));
#11444=CARTESIAN_POINT('',(-3.41,3.5,0.));
#11445=CARTESIAN_POINT('Origin',(-3.2,3.5,0.));
#11446=CARTESIAN_POINT('',(-3.41,3.5,1.));
#11447=CARTESIAN_POINT('',(-3.41,3.5,-0.1));
#11448=CARTESIAN_POINT('Origin',(-3.2,3.5,1.));
#11449=CARTESIAN_POINT('Origin',(3.2,5.5,-0.1));
#11450=CARTESIAN_POINT('',(2.99,5.5,0.));
#11451=CARTESIAN_POINT('Origin',(3.2,5.5,0.));
#11452=CARTESIAN_POINT('',(2.99,5.5,1.));
#11453=CARTESIAN_POINT('',(2.99,5.5,-0.1));
#11454=CARTESIAN_POINT('Origin',(3.2,5.5,1.));
#11455=CARTESIAN_POINT('Origin',(28.,10.,0.));
#11456=CARTESIAN_POINT('',(28.,10.,0.));
#11457=CARTESIAN_POINT('',(-5.,10.,0.));
#11458=CARTESIAN_POINT('',(28.,10.,0.));
#11459=CARTESIAN_POINT('',(-5.,10.,1.));
#11460=CARTESIAN_POINT('',(-5.,10.,0.));
#11461=CARTESIAN_POINT('',(28.,10.,1.));
#11462=CARTESIAN_POINT('',(28.,10.,1.));
#11463=CARTESIAN_POINT('',(28.,10.,0.));
#11464=CARTESIAN_POINT('Origin',(28.,-5.,0.));
#11465=CARTESIAN_POINT('',(28.,-5.,0.));
#11466=CARTESIAN_POINT('',(28.,-5.,0.));
#11467=CARTESIAN_POINT('',(28.,-5.,1.));
#11468=CARTESIAN_POINT('',(28.,-5.,1.));
#11469=CARTESIAN_POINT('',(28.,-5.,0.));
#11470=CARTESIAN_POINT('Origin',(-5.,-5.,0.));
#11471=CARTESIAN_POINT('',(-5.,-5.,0.));
#11472=CARTESIAN_POINT('',(-5.,-5.,0.));
#11473=CARTESIAN_POINT('',(-5.,-5.,1.));
#11474=CARTESIAN_POINT('',(-5.,-5.,1.));
#11475=CARTESIAN_POINT('',(-5.,-5.,0.));
#11476=CARTESIAN_POINT('Origin',(-5.,10.,0.));
#11477=CARTESIAN_POINT('',(-5.,10.,0.));
#11478=CARTESIAN_POINT('',(-5.,10.,1.));
#11479=CARTESIAN_POINT('Origin',(11.5,2.5,1.));
#11480=CARTESIAN_POINT('Origin',(11.5,2.5,0.));
#11481=CARTESIAN_POINT('',(0.,0.,0.));
#11482=CARTESIAN_POINT('Origin',(-3.,10.,-0.5));
#11483=CARTESIAN_POINT('',(-3.,10.,-0.5));
#11484=CARTESIAN_POINT('',(-5.,10.,-0.5));
#11485=CARTESIAN_POINT('',(-3.,10.,-0.5));
#11486=CARTESIAN_POINT('',(-5.,10.,0.));
#11487=CARTESIAN_POINT('',(-5.,10.,-0.5));
#11488=CARTESIAN_POINT('',(-3.,10.,0.));
#11489=CARTESIAN_POINT('',(-3.,10.,0.));
#11490=CARTESIAN_POINT('',(-3.,10.,-0.5));
#11491=CARTESIAN_POINT('Origin',(-3.,-5.,-0.5));
#11492=CARTESIAN_POINT('',(-3.,-5.,-0.5));
#11493=CARTESIAN_POINT('',(-3.,-5.,-0.5));
#11494=CARTESIAN_POINT('',(-3.,-5.,0.));
#11495=CARTESIAN_POINT('',(-3.,-5.,0.));
#11496=CARTESIAN_POINT('',(-3.,-5.,-0.5));
#11497=CARTESIAN_POINT('Origin',(-5.,-5.,-0.5));
#11498=CARTESIAN_POINT('',(-5.,-5.,-0.5));
#11499=CARTESIAN_POINT('',(-5.,-5.,-0.5));
#11500=CARTESIAN_POINT('',(-5.,-5.,0.));
#11501=CARTESIAN_POINT('',(-5.,-5.,0.));
#11502=CARTESIAN_POINT('',(-5.,-5.,-0.5));
#11503=CARTESIAN_POINT('Origin',(-5.,10.,-0.5));
#11504=CARTESIAN_POINT('',(-5.,10.,-0.5));
#11505=CARTESIAN_POINT('',(-5.,10.,0.));
#11506=CARTESIAN_POINT('Origin',(-4.,2.5,0.));
#11507=CARTESIAN_POINT('Origin',(-4.,2.5,-0.5));
#11508=CARTESIAN_POINT('',(0.,0.,0.));
#11509=CARTESIAN_POINT('Origin',(28.,10.,-0.5));
#11510=CARTESIAN_POINT('',(28.,10.,-0.5));
#11511=CARTESIAN_POINT('',(26.,10.,-0.5));
#11512=CARTESIAN_POINT('',(28.,10.,-0.5));
#11513=CARTESIAN_POINT('',(26.,10.,0.));
#11514=CARTESIAN_POINT('',(26.,10.,-0.5));
#11515=CARTESIAN_POINT('',(28.,10.,0.));
#11516=CARTESIAN_POINT('',(28.,10.,0.));
#11517=CARTESIAN_POINT('',(28.,10.,-0.5));
#11518=CARTESIAN_POINT('Origin',(28.,-5.,-0.5));
#11519=CARTESIAN_POINT('',(28.,-5.,-0.5));
#11520=CARTESIAN_POINT('',(28.,-5.,-0.5));
#11521=CARTESIAN_POINT('',(28.,-5.,0.));
#11522=CARTESIAN_POINT('',(28.,-5.,0.));
#11523=CARTESIAN_POINT('',(28.,-5.,-0.5));
#11524=CARTESIAN_POINT('Origin',(26.,-5.,-0.5));
#11525=CARTESIAN_POINT('',(26.,-5.,-0.5));
#11526=CARTESIAN_POINT('',(26.,-5.,-0.5));
#11527=CARTESIAN_POINT('',(26.,-5.,0.));
#11528=CARTESIAN_POINT('',(26.,-5.,0.));
#11529=CARTESIAN_POINT('',(26.,-5.,-0.5));
#11530=CARTESIAN_POINT('Origin',(26.,10.,-0.5));
#11531=CARTESIAN_POINT('',(26.,10.,-0.5));
#11532=CARTESIAN_POINT('',(26.,10.,0.));
#11533=CARTESIAN_POINT('Origin',(27.,2.5,0.));
#11534=CARTESIAN_POINT('Origin',(27.,2.5,-0.5));
#11535=CARTESIAN_POINT('',(0.,0.,0.));
#11536=CARTESIAN_POINT('Origin',(-2.6,3.4,11.));
#11537=CARTESIAN_POINT('',(-2.5,3.4,11.165));
#11538=CARTESIAN_POINT('Origin',(-2.5,3.4,11.));
#11539=CARTESIAN_POINT('',(-1.6,3.4,11.165));
#11540=CARTESIAN_POINT('',(-2.6,3.4,11.165));
#11541=CARTESIAN_POINT('Origin',(-1.6,3.4,11.));
#11542=CARTESIAN_POINT('Origin',(-1.6,3.4,11.));
#11543=CARTESIAN_POINT('Origin',(1.15,2.8,14.));
#11544=CARTESIAN_POINT('',(0.985,2.9,14.));
#11545=CARTESIAN_POINT('Origin',(1.15,2.9,14.));
#11546=CARTESIAN_POINT('',(0.985,3.9,14.));
#11547=CARTESIAN_POINT('',(0.985,2.8,14.));
#11548=CARTESIAN_POINT('Origin',(1.15,3.9,14.));
#11549=CARTESIAN_POINT('Origin',(-0.575,2.8,14.9959292143521));
#11550=CARTESIAN_POINT('',(-0.74,2.9,14.9959292143521));
#11551=CARTESIAN_POINT('Origin',(-0.575,2.9,14.9959292143521));
#11552=CARTESIAN_POINT('',(-0.74,3.9,14.9959292143521));
#11553=CARTESIAN_POINT('',(-0.74,2.8,14.9959292143521));
#11554=CARTESIAN_POINT('Origin',(-0.575,3.9,14.9959292143521));
#11555=CARTESIAN_POINT('Origin',(-0.575000000000001,2.8,13.0040707856479));
#11556=CARTESIAN_POINT('',(-0.74,2.9,13.0040707856479));
#11557=CARTESIAN_POINT('Origin',(-0.575000000000001,2.9,13.0040707856479));
#11558=CARTESIAN_POINT('',(-0.74,3.9,13.0040707856479));
#11559=CARTESIAN_POINT('',(-0.74,2.8,13.0040707856479));
#11560=CARTESIAN_POINT('Origin',(-0.575000000000001,3.9,13.0040707856479));
#11561=CARTESIAN_POINT('Origin',(0.,2.8,14.));
#11562=CARTESIAN_POINT('',(-0.505,2.9,14.));
#11563=CARTESIAN_POINT('Origin',(0.,2.9,14.));
#11564=CARTESIAN_POINT('',(-0.505,3.9,14.));
#11565=CARTESIAN_POINT('',(-0.505,2.8,14.));
#11566=CARTESIAN_POINT('Origin',(0.,3.9,14.));
#11567=CARTESIAN_POINT('Origin',(1.15,2.8,8.));
#11568=CARTESIAN_POINT('',(0.985,2.9,8.));
#11569=CARTESIAN_POINT('Origin',(1.15,2.9,8.));
#11570=CARTESIAN_POINT('',(0.985,3.9,8.));
#11571=CARTESIAN_POINT('',(0.985,2.8,8.));
#11572=CARTESIAN_POINT('Origin',(1.15,3.9,8.));
#11573=CARTESIAN_POINT('Origin',(-0.575,2.8,8.9959292143521));
#11574=CARTESIAN_POINT('',(-0.74,2.9,8.9959292143521));
#11575=CARTESIAN_POINT('Origin',(-0.575,2.9,8.9959292143521));
#11576=CARTESIAN_POINT('',(-0.74,3.9,8.9959292143521));
#11577=CARTESIAN_POINT('',(-0.74,2.8,8.9959292143521));
#11578=CARTESIAN_POINT('Origin',(-0.575,3.9,8.9959292143521));
#11579=CARTESIAN_POINT('Origin',(-0.575000000000001,2.8,7.0040707856479));
#11580=CARTESIAN_POINT('',(-0.74,2.9,7.0040707856479));
#11581=CARTESIAN_POINT('Origin',(-0.575000000000001,2.9,7.0040707856479));
#11582=CARTESIAN_POINT('',(-0.74,3.9,7.0040707856479));
#11583=CARTESIAN_POINT('',(-0.74,2.8,7.0040707856479));
#11584=CARTESIAN_POINT('Origin',(-0.575000000000001,3.9,7.0040707856479));
#11585=CARTESIAN_POINT('Origin',(0.,2.8,8.));
#11586=CARTESIAN_POINT('',(-0.505,2.9,8.));
#11587=CARTESIAN_POINT('Origin',(0.,2.9,8.));
#11588=CARTESIAN_POINT('',(-0.505,3.9,8.));
#11589=CARTESIAN_POINT('',(-0.505,2.8,8.));
#11590=CARTESIAN_POINT('Origin',(0.,3.9,8.));
#11591=CARTESIAN_POINT('Origin',(3.2,3.5,0.9));
#11592=CARTESIAN_POINT('',(2.925,3.5,1.));
#11593=CARTESIAN_POINT('Origin',(3.2,3.5,1.));
#11594=CARTESIAN_POINT('',(2.925,3.5,1.8));
#11595=CARTESIAN_POINT('',(2.925,3.5,0.9));
#11596=CARTESIAN_POINT('Origin',(3.2,3.5,1.8));
#11597=CARTESIAN_POINT('Origin',(-3.2,5.5,0.9));
#11598=CARTESIAN_POINT('',(-3.475,5.5,1.));
#11599=CARTESIAN_POINT('Origin',(-3.2,5.5,1.));
#11600=CARTESIAN_POINT('',(-3.475,5.5,1.8));
#11601=CARTESIAN_POINT('',(-3.475,5.5,0.9));
#11602=CARTESIAN_POINT('Origin',(-3.2,5.5,1.8));
#11603=CARTESIAN_POINT('Origin',(-3.2,3.5,0.9));
#11604=CARTESIAN_POINT('',(-3.475,3.5,1.));
#11605=CARTESIAN_POINT('Origin',(-3.2,3.5,1.));
#11606=CARTESIAN_POINT('',(-3.475,3.5,1.8));
#11607=CARTESIAN_POINT('',(-3.475,3.5,0.9));
#11608=CARTESIAN_POINT('Origin',(-3.2,3.5,1.8));
#11609=CARTESIAN_POINT('Origin',(3.2,5.5,0.9));
#11610=CARTESIAN_POINT('',(2.925,5.5,1.));
#11611=CARTESIAN_POINT('Origin',(3.2,5.5,1.));
#11612=CARTESIAN_POINT('',(2.925,5.5,1.8));
#11613=CARTESIAN_POINT('',(2.925,5.5,0.9));
#11614=CARTESIAN_POINT('Origin',(3.2,5.5,1.8));
#11615=CARTESIAN_POINT('Origin',(-4.,2.9,1.8));
#11616=CARTESIAN_POINT('',(-2.5,3.9,1.8));
#11617=CARTESIAN_POINT('',(-2.5,2.9,1.8));
#11618=CARTESIAN_POINT('',(-2.5,3.9,1.8));
#11619=CARTESIAN_POINT('',(2.5,3.9,1.8));
#11620=CARTESIAN_POINT('',(2.5,3.9,1.8));
#11621=CARTESIAN_POINT('',(2.5,2.9,1.8));
#11622=CARTESIAN_POINT('',(2.5,2.9,1.8));
#11623=CARTESIAN_POINT('',(4.,2.9,1.8));
#11624=CARTESIAN_POINT('',(4.,2.9,1.8));
#11625=CARTESIAN_POINT('',(4.,6.9,1.8));
#11626=CARTESIAN_POINT('',(4.,2.9,1.8));
#11627=CARTESIAN_POINT('',(-4.,6.9,1.8));
#11628=CARTESIAN_POINT('',(4.,6.9,1.8));
#11629=CARTESIAN_POINT('',(-4.,2.9,1.8));
#11630=CARTESIAN_POINT('',(-4.,2.9,1.8));
#11631=CARTESIAN_POINT('',(4.,2.9,1.8));
#11632=CARTESIAN_POINT('Origin',(-4.,2.9,1.));
#11633=CARTESIAN_POINT('',(-4.,2.9,1.));
#11634=CARTESIAN_POINT('',(-4.,2.9,1.8));
#11635=CARTESIAN_POINT('',(-4.,6.9,1.));
#11636=CARTESIAN_POINT('',(-4.,6.9,1.8));
#11637=CARTESIAN_POINT('',(-4.,2.9,1.));
#11638=CARTESIAN_POINT('Origin',(4.,2.9,1.));
#11639=CARTESIAN_POINT('',(4.,2.9,1.));
#11640=CARTESIAN_POINT('',(-4.,2.9,1.));
#11641=CARTESIAN_POINT('',(4.,6.9,1.));
#11642=CARTESIAN_POINT('',(-4.,6.9,1.));
#11643=CARTESIAN_POINT('',(4.,2.9,1.));
#11644=CARTESIAN_POINT('Origin',(4.,2.9,1.8));
#11645=CARTESIAN_POINT('',(4.,2.9,1.));
#11646=CARTESIAN_POINT('',(4.,6.9,1.));
#11647=CARTESIAN_POINT('Origin',(0.,6.9,1.4));
#11648=CARTESIAN_POINT('Origin',(2.5,3.9,1.8));
#11649=CARTESIAN_POINT('',(-2.5,3.9,17.));
#11650=CARTESIAN_POINT('',(-2.5,3.9,1.8));
#11651=CARTESIAN_POINT('',(2.5,3.9,17.));
#11652=CARTESIAN_POINT('',(2.5,3.9,17.));
#11653=CARTESIAN_POINT('',(2.5,3.9,1.8));
#11654=CARTESIAN_POINT('Origin',(2.5,2.9,1.8));
#11655=CARTESIAN_POINT('',(2.5,2.9,17.));
#11656=CARTESIAN_POINT('',(2.5,2.9,17.));
#11657=CARTESIAN_POINT('',(2.5,2.9,1.8));
#11658=CARTESIAN_POINT('Origin',(-2.5,2.9,1.8));
#11659=CARTESIAN_POINT('',(-2.5,2.9,17.));
#11660=CARTESIAN_POINT('',(-2.5,2.9,17.));
#11661=CARTESIAN_POINT('',(-2.5,2.9,1.8));
#11662=CARTESIAN_POINT('Origin',(-2.5,3.9,1.8));
#11663=CARTESIAN_POINT('',(-2.5,3.9,17.));
#11664=CARTESIAN_POINT('Origin',(0.,3.4,17.));
#11665=CARTESIAN_POINT('',(0.,0.,0.));
#11666=CARTESIAN_POINT('Origin',(0.,-4.1,8.));
#11667=CARTESIAN_POINT('',(-0.165,-4.,8.));
#11668=CARTESIAN_POINT('Origin',(0.,-4.,8.));
#11669=CARTESIAN_POINT('',(-0.165,-2.4,8.));
#11670=CARTESIAN_POINT('',(-0.165,-4.1,8.));
#11671=CARTESIAN_POINT('Origin',(0.,-2.4,8.));
#11672=CARTESIAN_POINT('Origin',(0.,-2.4,8.));
#11673=CARTESIAN_POINT('Origin',(1.15,2.4,8.));
#11674=CARTESIAN_POINT('',(0.925,2.5,8.));
#11675=CARTESIAN_POINT('Origin',(1.15,2.5,8.));
#11676=CARTESIAN_POINT('',(0.925,2.9,8.));
#11677=CARTESIAN_POINT('',(0.925,2.4,8.));
#11678=CARTESIAN_POINT('Origin',(1.15,2.9,8.));
#11679=CARTESIAN_POINT('Origin',(-0.575,2.4,8.9959292143521));
#11680=CARTESIAN_POINT('',(-0.8,2.5,8.9959292143521));
#11681=CARTESIAN_POINT('Origin',(-0.575,2.5,8.9959292143521));
#11682=CARTESIAN_POINT('',(-0.8,2.9,8.9959292143521));
#11683=CARTESIAN_POINT('',(-0.8,2.4,8.9959292143521));
#11684=CARTESIAN_POINT('Origin',(-0.575,2.9,8.9959292143521));
#11685=CARTESIAN_POINT('Origin',(-0.575000000000001,2.4,7.0040707856479));
#11686=CARTESIAN_POINT('',(-0.8,2.5,7.0040707856479));
#11687=CARTESIAN_POINT('Origin',(-0.575000000000001,2.5,7.0040707856479));
#11688=CARTESIAN_POINT('',(-0.8,2.9,7.0040707856479));
#11689=CARTESIAN_POINT('',(-0.8,2.4,7.0040707856479));
#11690=CARTESIAN_POINT('Origin',(-0.575000000000001,2.9,7.0040707856479));
#11691=CARTESIAN_POINT('Origin',(0.,2.9,8.));
#11692=CARTESIAN_POINT('',(-1.5,2.9,8.));
#11693=CARTESIAN_POINT('Origin',(0.,2.9,8.));
#11694=CARTESIAN_POINT('',(-0.5,2.9,8.));
#11695=CARTESIAN_POINT('Origin',(0.,2.9,8.));
#11696=CARTESIAN_POINT('Origin',(0.,2.5,8.));
#11697=CARTESIAN_POINT('',(-1.5,2.5,8.));
#11698=CARTESIAN_POINT('Origin',(0.,2.5,8.));
#11699=CARTESIAN_POINT('',(-0.5,2.5,8.));
#11700=CARTESIAN_POINT('Origin',(0.,2.5,8.));
#11701=CARTESIAN_POINT('Origin',(0.,2.5,8.));
#11702=CARTESIAN_POINT('',(-1.5,2.5,8.));
#11703=CARTESIAN_POINT('Origin',(0.,-4.,8.));
#11704=CARTESIAN_POINT('',(-0.5,-4.,8.));
#11705=CARTESIAN_POINT('',(-0.5,-4.,8.));
#11706=CARTESIAN_POINT('Origin',(0.,-4.,8.));
#11707=CARTESIAN_POINT('Origin',(0.,-4.,8.));
#11708=CARTESIAN_POINT('',(-0.5,3.9,8.));
#11709=CARTESIAN_POINT('Origin',(0.,3.9,8.));
#11710=CARTESIAN_POINT('',(-0.5,-4.,8.));
#11711=CARTESIAN_POINT('Origin',(0.,3.9,8.));
#11712=CARTESIAN_POINT('Origin',(0.,-4.,8.));
#11713=CARTESIAN_POINT('',(0.,0.,0.));
#11714=CARTESIAN_POINT('Origin',(0.,-0.15,8.));
#11715=CARTESIAN_POINT('',(-0.505,0.15,8.));
#11716=CARTESIAN_POINT('Origin',(0.,0.15,8.));
#11717=CARTESIAN_POINT('',(-0.505,-0.15,8.));
#11718=CARTESIAN_POINT('',(-0.505,-0.15,8.));
#11719=CARTESIAN_POINT('Origin',(0.,-0.15,8.));
#11720=CARTESIAN_POINT('Origin',(0.,-0.15,8.));
#11721=CARTESIAN_POINT('',(-0.7,0.15,8.));
#11722=CARTESIAN_POINT('Origin',(0.,0.15,8.));
#11723=CARTESIAN_POINT('',(-0.7,-0.15,8.));
#11724=CARTESIAN_POINT('',(-0.7,-0.15,8.));
#11725=CARTESIAN_POINT('Origin',(0.,-0.15,8.));
#11726=CARTESIAN_POINT('Origin',(0.,0.15,8.));
#11727=CARTESIAN_POINT('Origin',(0.,-0.15,8.));
#11728=CARTESIAN_POINT('',(0.,0.,0.));
#11729=CARTESIAN_POINT('Origin',(0.,1.05,8.));
#11730=CARTESIAN_POINT('',(-0.505,2.5,8.));
#11731=CARTESIAN_POINT('Origin',(0.,2.5,8.));
#11732=CARTESIAN_POINT('',(-0.505,1.05,8.));
#11733=CARTESIAN_POINT('',(-0.505,1.05,8.));
#11734=CARTESIAN_POINT('Origin',(0.,1.05,8.));
#11735=CARTESIAN_POINT('Origin',(0.,1.05,8.));
#11736=CARTESIAN_POINT('',(-0.7,2.5,8.));
#11737=CARTESIAN_POINT('Origin',(0.,2.5,8.));
#11738=CARTESIAN_POINT('',(-0.7,1.05,8.));
#11739=CARTESIAN_POINT('',(-0.7,1.05,8.));
#11740=CARTESIAN_POINT('Origin',(0.,1.05,8.));
#11741=CARTESIAN_POINT('Origin',(0.,2.5,8.));
#11742=CARTESIAN_POINT('Origin',(0.,1.05,8.));
#11743=CARTESIAN_POINT('',(0.,0.,0.));
#11744=CARTESIAN_POINT('Origin',(0.,-4.,8.));
#11745=CARTESIAN_POINT('',(-0.505,-1.05,8.));
#11746=CARTESIAN_POINT('Origin',(0.,-1.05,8.));
#11747=CARTESIAN_POINT('',(-0.505,-4.,8.));
#11748=CARTESIAN_POINT('',(-0.505,-4.,8.));
#11749=CARTESIAN_POINT('Origin',(0.,-4.,8.));
#11750=CARTESIAN_POINT('Origin',(0.,-4.,8.));
#11751=CARTESIAN_POINT('',(-0.7,-1.05,8.));
#11752=CARTESIAN_POINT('Origin',(0.,-1.05,8.));
#11753=CARTESIAN_POINT('',(-0.7,-4.,8.));
#11754=CARTESIAN_POINT('',(-0.7,-4.,8.));
#11755=CARTESIAN_POINT('Origin',(0.,-4.,8.));
#11756=CARTESIAN_POINT('Origin',(0.,-1.05,8.));
#11757=CARTESIAN_POINT('Origin',(0.,-4.,8.));
#11758=CARTESIAN_POINT('',(0.,0.,0.));
#11759=CARTESIAN_POINT('Origin',(0.,-4.2,8.));
#11760=CARTESIAN_POINT('',(-0.225,-4.,8.));
#11761=CARTESIAN_POINT('Origin',(0.,-4.,8.));
#11762=CARTESIAN_POINT('',(-0.225,-4.2,8.));
#11763=CARTESIAN_POINT('',(-0.225,-4.2,8.));
#11764=CARTESIAN_POINT('Origin',(0.,-4.2,8.));
#11765=CARTESIAN_POINT('Origin',(0.,-4.2,8.));
#11766=CARTESIAN_POINT('',(-0.9,-4.,8.));
#11767=CARTESIAN_POINT('Origin',(0.,-4.,8.));
#11768=CARTESIAN_POINT('',(-0.9,-4.2,8.));
#11769=CARTESIAN_POINT('',(-0.9,-4.2,8.));
#11770=CARTESIAN_POINT('Origin',(0.,-4.2,8.));
#11771=CARTESIAN_POINT('Origin',(0.,-4.,8.));
#11772=CARTESIAN_POINT('Origin',(0.,-4.2,8.));
#11773=CARTESIAN_POINT('',(0.,0.,0.));
#11774=CARTESIAN_POINT('Origin',(0.,-1.7,14.));
#11775=CARTESIAN_POINT('',(-0.165,-1.6,14.));
#11776=CARTESIAN_POINT('Origin',(0.,-1.6,14.));
#11777=CARTESIAN_POINT('',(-0.165,0.,14.));
#11778=CARTESIAN_POINT('',(-0.165,-1.7,14.));
#11779=CARTESIAN_POINT('Origin',(0.,0.,14.));
#11780=CARTESIAN_POINT('Origin',(0.,0.,14.));
#11781=CARTESIAN_POINT('Origin',(1.15,2.4,14.));
#11782=CARTESIAN_POINT('',(0.925,2.5,14.));
#11783=CARTESIAN_POINT('Origin',(1.15,2.5,14.));
#11784=CARTESIAN_POINT('',(0.925,2.9,14.));
#11785=CARTESIAN_POINT('',(0.925,2.4,14.));
#11786=CARTESIAN_POINT('Origin',(1.15,2.9,14.));
#11787=CARTESIAN_POINT('Origin',(-0.575,2.4,14.9959292143521));
#11788=CARTESIAN_POINT('',(-0.8,2.5,14.9959292143521));
#11789=CARTESIAN_POINT('Origin',(-0.575,2.5,14.9959292143521));
#11790=CARTESIAN_POINT('',(-0.8,2.9,14.9959292143521));
#11791=CARTESIAN_POINT('',(-0.8,2.4,14.9959292143521));
#11792=CARTESIAN_POINT('Origin',(-0.575,2.9,14.9959292143521));
#11793=CARTESIAN_POINT('Origin',(-0.575000000000001,2.4,13.0040707856479));
#11794=CARTESIAN_POINT('',(-0.8,2.5,13.0040707856479));
#11795=CARTESIAN_POINT('Origin',(-0.575000000000001,2.5,13.0040707856479));
#11796=CARTESIAN_POINT('',(-0.8,2.9,13.0040707856479));
#11797=CARTESIAN_POINT('',(-0.8,2.4,13.0040707856479));
#11798=CARTESIAN_POINT('Origin',(-0.575000000000001,2.9,13.0040707856479));
#11799=CARTESIAN_POINT('Origin',(0.,2.9,14.));
#11800=CARTESIAN_POINT('',(-1.5,2.9,14.));
#11801=CARTESIAN_POINT('Origin',(0.,2.9,14.));
#11802=CARTESIAN_POINT('',(-0.5,2.9,14.));
#11803=CARTESIAN_POINT('Origin',(0.,2.9,14.));
#11804=CARTESIAN_POINT('Origin',(0.,2.5,14.));
#11805=CARTESIAN_POINT('',(-1.5,2.5,14.));
#11806=CARTESIAN_POINT('Origin',(0.,2.5,14.));
#11807=CARTESIAN_POINT('',(-0.5,2.5,14.));
#11808=CARTESIAN_POINT('Origin',(0.,2.5,14.));
#11809=CARTESIAN_POINT('Origin',(0.,2.5,14.));
#11810=CARTESIAN_POINT('',(-1.5,2.5,14.));
#11811=CARTESIAN_POINT('Origin',(0.,-1.6,14.));
#11812=CARTESIAN_POINT('',(-0.5,-1.6,14.));
#11813=CARTESIAN_POINT('',(-0.5,-1.6,14.));
#11814=CARTESIAN_POINT('Origin',(0.,-1.6,14.));
#11815=CARTESIAN_POINT('Origin',(0.,-1.6,14.));
#11816=CARTESIAN_POINT('',(-0.5,3.9,14.));
#11817=CARTESIAN_POINT('Origin',(0.,3.9,14.));
#11818=CARTESIAN_POINT('',(-0.5,-1.6,14.));
#11819=CARTESIAN_POINT('Origin',(0.,3.9,14.));
#11820=CARTESIAN_POINT('Origin',(0.,-1.6,14.));
#11821=CARTESIAN_POINT('',(0.,0.,0.));
#11822=CARTESIAN_POINT('Origin',(0.,-0.15,14.));
#11823=CARTESIAN_POINT('',(-0.505,0.15,14.));
#11824=CARTESIAN_POINT('Origin',(0.,0.15,14.));
#11825=CARTESIAN_POINT('',(-0.505,-0.15,14.));
#11826=CARTESIAN_POINT('',(-0.505,-0.15,14.));
#11827=CARTESIAN_POINT('Origin',(0.,-0.15,14.));
#11828=CARTESIAN_POINT('Origin',(0.,-0.15,14.));
#11829=CARTESIAN_POINT('',(-0.7,0.15,14.));
#11830=CARTESIAN_POINT('Origin',(0.,0.15,14.));
#11831=CARTESIAN_POINT('',(-0.7,-0.15,14.));
#11832=CARTESIAN_POINT('',(-0.7,-0.15,14.));
#11833=CARTESIAN_POINT('Origin',(0.,-0.15,14.));
#11834=CARTESIAN_POINT('Origin',(0.,0.15,14.));
#11835=CARTESIAN_POINT('Origin',(0.,-0.15,14.));
#11836=CARTESIAN_POINT('',(0.,0.,0.));
#11837=CARTESIAN_POINT('Origin',(0.,1.05,14.));
#11838=CARTESIAN_POINT('',(-0.505,2.5,14.));
#11839=CARTESIAN_POINT('Origin',(0.,2.5,14.));
#11840=CARTESIAN_POINT('',(-0.505,1.05,14.));
#11841=CARTESIAN_POINT('',(-0.505,1.05,14.));
#11842=CARTESIAN_POINT('Origin',(0.,1.05,14.));
#11843=CARTESIAN_POINT('Origin',(0.,1.05,14.));
#11844=CARTESIAN_POINT('',(-0.7,2.5,14.));
#11845=CARTESIAN_POINT('Origin',(0.,2.5,14.));
#11846=CARTESIAN_POINT('',(-0.7,1.05,14.));
#11847=CARTESIAN_POINT('',(-0.7,1.05,14.));
#11848=CARTESIAN_POINT('Origin',(0.,1.05,14.));
#11849=CARTESIAN_POINT('Origin',(0.,2.5,14.));
#11850=CARTESIAN_POINT('Origin',(0.,1.05,14.));
#11851=CARTESIAN_POINT('',(0.,0.,0.));
#11852=CARTESIAN_POINT('Origin',(0.,-1.6,14.));
#11853=CARTESIAN_POINT('',(-0.505,-1.05,14.));
#11854=CARTESIAN_POINT('Origin',(0.,-1.05,14.));
#11855=CARTESIAN_POINT('',(-0.505,-1.6,14.));
#11856=CARTESIAN_POINT('',(-0.505,-1.6,14.));
#11857=CARTESIAN_POINT('Origin',(0.,-1.6,14.));
#11858=CARTESIAN_POINT('Origin',(0.,-1.6,14.));
#11859=CARTESIAN_POINT('',(-0.7,-1.05,14.));
#11860=CARTESIAN_POINT('Origin',(0.,-1.05,14.));
#11861=CARTESIAN_POINT('',(-0.7,-1.6,14.));
#11862=CARTESIAN_POINT('',(-0.7,-1.6,14.));
#11863=CARTESIAN_POINT('Origin',(0.,-1.6,14.));
#11864=CARTESIAN_POINT('Origin',(0.,-1.05,14.));
#11865=CARTESIAN_POINT('Origin',(0.,-1.6,14.));
#11866=CARTESIAN_POINT('',(0.,0.,0.));
#11867=CARTESIAN_POINT('Origin',(0.,-1.8,14.));
#11868=CARTESIAN_POINT('',(-0.225,-1.6,14.));
#11869=CARTESIAN_POINT('Origin',(0.,-1.6,14.));
#11870=CARTESIAN_POINT('',(-0.225,-1.8,14.));
#11871=CARTESIAN_POINT('',(-0.225,-1.8,14.));
#11872=CARTESIAN_POINT('Origin',(0.,-1.8,14.));
#11873=CARTESIAN_POINT('Origin',(0.,-1.8,14.));
#11874=CARTESIAN_POINT('',(-0.9,-1.6,14.));
#11875=CARTESIAN_POINT('Origin',(0.,-1.6,14.));
#11876=CARTESIAN_POINT('',(-0.9,-1.8,14.));
#11877=CARTESIAN_POINT('',(-0.9,-1.8,14.));
#11878=CARTESIAN_POINT('Origin',(0.,-1.8,14.));
#11879=CARTESIAN_POINT('Origin',(0.,-1.6,14.));
#11880=CARTESIAN_POINT('Origin',(0.,-1.8,14.));
#11881=CARTESIAN_POINT('',(0.,0.,0.));
#11882=CARTESIAN_POINT('Origin',(-3.6,3.4,11.));
#11883=CARTESIAN_POINT('',(-3.5,3.4,11.225));
#11884=CARTESIAN_POINT('Origin',(-3.5,3.4,11.));
#11885=CARTESIAN_POINT('',(-2.5,3.4,11.225));
#11886=CARTESIAN_POINT('',(-3.6,3.4,11.225));
#11887=CARTESIAN_POINT('Origin',(-2.5,3.4,11.));
#11888=CARTESIAN_POINT('Origin',(0.8,-2.2,10.4));
#11889=CARTESIAN_POINT('',(0.73,-2.2,10.5));
#11890=CARTESIAN_POINT('Origin',(0.8,-2.2,10.5));
#11891=CARTESIAN_POINT('',(0.73,-2.2,11.5));
#11892=CARTESIAN_POINT('',(0.73,-2.2,10.4));
#11893=CARTESIAN_POINT('Origin',(0.8,-2.2,11.5));
#11894=CARTESIAN_POINT('Origin',(0.4,-2.6,10.5));
#11895=CARTESIAN_POINT('',(0.4,-2.6,10.9));
#11896=CARTESIAN_POINT('',(0.4,-1.8,10.9));
#11897=CARTESIAN_POINT('',(0.4,-2.6,10.9));
#11898=CARTESIAN_POINT('',(0.4,-2.6,11.5));
#11899=CARTESIAN_POINT('',(0.4,-2.6,11.5));
#11900=CARTESIAN_POINT('',(0.4,-1.8,11.5));
#11901=CARTESIAN_POINT('',(0.4,-2.6,11.5));
#11902=CARTESIAN_POINT('',(0.4,-1.8,11.5));
#11903=CARTESIAN_POINT('Origin',(0.4,-2.6,11.5));
#11904=CARTESIAN_POINT('',(1.2,-2.6,11.5));
#11905=CARTESIAN_POINT('',(1.2,-2.6,11.5));
#11906=CARTESIAN_POINT('',(1.2,-1.8,11.5));
#11907=CARTESIAN_POINT('',(1.2,-2.6,11.5));
#11908=CARTESIAN_POINT('',(1.2,-1.8,11.5));
#11909=CARTESIAN_POINT('Origin',(-3.5,-2.6,10.5));
#11910=CARTESIAN_POINT('',(-2.5,-2.6,10.9));
#11911=CARTESIAN_POINT('',(1.2,-2.6,10.9));
#11912=CARTESIAN_POINT('',(-2.5,-2.6,11.5));
#11913=CARTESIAN_POINT('',(-2.5,-2.6,10.5));
#11914=CARTESIAN_POINT('',(-3.5,-2.6,11.5));
#11915=CARTESIAN_POINT('',(-3.5,-2.6,11.5));
#11916=CARTESIAN_POINT('',(-3.5,-2.6,10.5));
#11917=CARTESIAN_POINT('',(-3.5,-2.6,10.5));
#11918=CARTESIAN_POINT('',(1.2,-2.6,10.5));
#11919=CARTESIAN_POINT('',(-3.5,-2.6,10.5));
#11920=CARTESIAN_POINT('',(1.2,-2.6,10.5));
#11921=CARTESIAN_POINT('Origin',(-3.5,-2.6,10.9));
#11922=CARTESIAN_POINT('',(-2.5,-1.8,10.9));
#11923=CARTESIAN_POINT('',(1.2,-1.8,10.9));
#11924=CARTESIAN_POINT('',(-2.5,-2.6,10.9));
#11925=CARTESIAN_POINT('Origin',(-1.15,-1.8,10.7));
#11926=CARTESIAN_POINT('',(1.2,-1.8,10.5));
#11927=CARTESIAN_POINT('',(-2.5,-1.8,10.5));
#11928=CARTESIAN_POINT('',(-3.5,-1.8,10.5));
#11929=CARTESIAN_POINT('',(-2.5,-1.8,10.6));
#11930=CARTESIAN_POINT('',(1.2,-1.8,10.5));
#11931=CARTESIAN_POINT('Origin',(1.2,-2.6,10.9));
#11932=CARTESIAN_POINT('',(1.2,-2.6,10.5));
#11933=CARTESIAN_POINT('Origin',(-3.5,3.9,10.5));
#11934=CARTESIAN_POINT('',(-3.5,3.9,10.5));
#11935=CARTESIAN_POINT('',(-3.5,3.9,10.5));
#11936=CARTESIAN_POINT('',(-3.5,3.9,11.5));
#11937=CARTESIAN_POINT('',(-3.5,3.9,11.5));
#11938=CARTESIAN_POINT('',(-3.5,3.9,10.5));
#11939=CARTESIAN_POINT('Origin',(-2.5,3.9,10.5));
#11940=CARTESIAN_POINT('',(-2.5,3.9,10.5));
#11941=CARTESIAN_POINT('',(-2.5,3.9,10.5));
#11942=CARTESIAN_POINT('',(-2.5,3.9,11.5));
#11943=CARTESIAN_POINT('',(-2.5,3.9,11.5));
#11944=CARTESIAN_POINT('',(-2.5,3.9,10.5));
#11945=CARTESIAN_POINT('Origin',(-2.5,-2.6,10.5));
#11946=CARTESIAN_POINT('',(-2.5,-2.6,10.5));
#11947=CARTESIAN_POINT('',(-2.5,-2.6,11.5));
#11948=CARTESIAN_POINT('Origin',(-3.,0.65,11.5));
#11949=CARTESIAN_POINT('Origin',(-3.,0.65,10.5));
#11950=CARTESIAN_POINT('',(0.,0.,0.));
#11951=CARTESIAN_POINT('Origin',(0.8,-3.4,8.));
#11952=CARTESIAN_POINT('',(4.,-3.4,8.06));
#11953=CARTESIAN_POINT('Origin',(4.,-3.4,8.));
#11954=CARTESIAN_POINT('',(0.799999999999999,-3.4,8.06));
#11955=CARTESIAN_POINT('',(0.8,-3.4,8.06));
#11956=CARTESIAN_POINT('',(0.8,-3.45981204140764,7.99525450712245));
#11957=CARTESIAN_POINT('Origin',(0.8,-3.4,8.));
#11958=CARTESIAN_POINT('',(0.857757769669024,-3.39074044575272,7.94071880015435));
#11959=CARTESIAN_POINT('Ctrl Pts',(0.857757769669022,-3.39074044575271,
7.94071880015434));
#11960=CARTESIAN_POINT('Ctrl Pts',(0.857868134836737,-3.3922890292717,7.94047691582781));
#11961=CARTESIAN_POINT('Ctrl Pts',(0.857921908329668,-3.39385496848479,
7.94029447157442));
#11962=CARTESIAN_POINT('Ctrl Pts',(0.857899468660573,-3.401217652612,7.93973268518719));
#11963=CARTESIAN_POINT('Ctrl Pts',(0.857099131366584,-3.40693773045843,
7.94013905492094));
#11964=CARTESIAN_POINT('Ctrl Pts',(0.853922333121985,-3.41863574050482,
7.94261529275599));
#11965=CARTESIAN_POINT('Ctrl Pts',(0.851411692482855,-3.42433770210915,
7.94484920249294));
#11966=CARTESIAN_POINT('Ctrl Pts',(0.844348873784965,-3.43603698949541,
7.95142983480112));
#11967=CARTESIAN_POINT('Ctrl Pts',(0.83945370863678,-3.44153123637203,7.95616729134823));
#11968=CARTESIAN_POINT('Ctrl Pts',(0.829171203288947,-3.45001457070346,
7.96624704549874));
#11969=CARTESIAN_POINT('Ctrl Pts',(0.82379008497386,-3.45317277823043,7.97157628615011));
#11970=CARTESIAN_POINT('Ctrl Pts',(0.812442480882928,-3.45783692899872,
7.98285013462503));
#11971=CARTESIAN_POINT('Ctrl Pts',(0.80639623862599,-3.45926990278519,7.98887603141664));
#11972=CARTESIAN_POINT('Ctrl Pts',(0.800230800143543,-3.45979344585912,
7.9950243425463));
#11973=CARTESIAN_POINT('Ctrl Pts',(0.800115406102298,-3.45980291021815,
7.99513941790037));
#11974=CARTESIAN_POINT('Ctrl Pts',(0.799999999999999,-3.45981204140764,
7.99525450712243));
#11975=CARTESIAN_POINT('',(0.8,-3.34018795859236,8.00474549287757));
#11976=CARTESIAN_POINT('Ctrl Pts',(0.8,-3.34018795859236,8.00474549287757));
#11977=CARTESIAN_POINT('Ctrl Pts',(0.800115406079139,-3.3401788320092,8.00463046171348));
#11978=CARTESIAN_POINT('Ctrl Pts',(0.800230800092475,-3.34017003627816,
8.0045153917222));
#11979=CARTESIAN_POINT('Ctrl Pts',(0.810811727464239,-3.33939379801257,
7.99395951069901));
#11980=CARTESIAN_POINT('Ctrl Pts',(0.820900841739028,-3.34136574707449,
7.98346560010985));
#11981=CARTESIAN_POINT('Ctrl Pts',(0.836664447625529,-3.34957747484304,
7.96642056687488));
#11982=CARTESIAN_POINT('Ctrl Pts',(0.842584279376725,-3.35471818663018,
7.95976549836209));
#11983=CARTESIAN_POINT('Ctrl Pts',(0.850737922589237,-3.36590371591375,
7.95021852968304));
#11984=CARTESIAN_POINT('Ctrl Pts',(0.853638109640398,-3.37164357089127,
7.94665881249463));
#11985=CARTESIAN_POINT('Ctrl Pts',(0.856693627441668,-3.38219046561222,
7.94254333724378));
#11986=CARTESIAN_POINT('Ctrl Pts',(0.857448232148212,-3.38639718498341,
7.9413972050923));
#11987=CARTESIAN_POINT('Ctrl Pts',(0.857757769669022,-3.39074044575271,
7.94071880015434));
#11988=CARTESIAN_POINT('Origin',(0.8,-3.4,8.));
#11989=CARTESIAN_POINT('Origin',(4.,-3.4,8.));
#11990=CARTESIAN_POINT('Origin',(0.8,-3.4,8.));
#11991=CARTESIAN_POINT('',(0.8,-3.4,8.));
#11992=CARTESIAN_POINT('Origin',(0.8,-3.4,8.));
#11993=CARTESIAN_POINT('Origin',(0.8,-3.4,8.));
#11994=CARTESIAN_POINT('Origin',(0.8,-2.2,8.));
#11995=CARTESIAN_POINT('',(0.74,-2.2,11.));
#11996=CARTESIAN_POINT('Origin',(0.8,-2.2,11.));
#11997=CARTESIAN_POINT('',(0.739999999999999,-2.2,8.41884281581389));
#11998=CARTESIAN_POINT('',(0.74,-2.2,8.));
#11999=CARTESIAN_POINT('',(0.859999911467078,-2.20010307251212,8.));
#12000=CARTESIAN_POINT('Ctrl Pts',(0.859999911467078,-2.20010307251221,
8.));
#12001=CARTESIAN_POINT('Ctrl Pts',(0.859999136901991,-2.20055395738578,
8.00090497885833));
#12002=CARTESIAN_POINT('Ctrl Pts',(0.859993279965474,-2.20100479566276,
8.00180978698512));
#12003=CARTESIAN_POINT('Ctrl Pts',(0.859613264338125,-2.21666553404949,
8.03325602937855));
#12004=CARTESIAN_POINT('Ctrl Pts',(0.853474853505761,-2.23105407285076,
8.06256859999788));
#12005=CARTESIAN_POINT('Ctrl Pts',(0.838027444543347,-2.24696762823943,
8.12558745018579));
#12006=CARTESIAN_POINT('Ctrl Pts',(0.832681318070563,-2.25065802014274,
8.14673824214296));
#12007=CARTESIAN_POINT('Ctrl Pts',(0.825757894768706,-2.25422415942331,
8.17441882347885));
#12008=CARTESIAN_POINT('Ctrl Pts',(0.824032187048781,-2.25500826562799,
8.18131842676915));
#12009=CARTESIAN_POINT('Ctrl Pts',(0.821583106170439,-2.25598907832281,
8.1910847498449));
#12010=CARTESIAN_POINT('Ctrl Pts',(0.820858026692738,-2.25626310384707,
8.19397291910405));
#12011=CARTESIAN_POINT('Ctrl Pts',(0.819663731786288,-2.2566884878246,8.19872186244263));
#12012=CARTESIAN_POINT('Ctrl Pts',(0.819194803735207,-2.25684895568773,
8.20058440860189));
#12013=CARTESIAN_POINT('Ctrl Pts',(0.818201492584122,-2.25717525350113,
8.20452431789242));
#12014=CARTESIAN_POINT('Ctrl Pts',(0.817676638293826,-2.25733966745791,
8.20660292114951));
#12015=CARTESIAN_POINT('Ctrl Pts',(0.816410515141555,-2.25771734508197,
8.2116077883401));
#12016=CARTESIAN_POINT('Ctrl Pts',(0.815667569715253,-2.25792338856219,
8.21453683995452));
#12017=CARTESIAN_POINT('Ctrl Pts',(0.813121121086004,-2.25857725854118,
8.22454278593531));
#12018=CARTESIAN_POINT('Ctrl Pts',(0.811298366698271,-2.25895601380967,
8.23164788351326));
#12019=CARTESIAN_POINT('Ctrl Pts',(0.805508922328413,-2.25988040695531,
8.25394436711295));
#12020=CARTESIAN_POINT('Ctrl Pts',(0.801392906371853,-2.26013248433115,
8.26939428603274));
#12021=CARTESIAN_POINT('Ctrl Pts',(0.787077992513295,-2.25945702001813,
8.32085142392661));
#12022=CARTESIAN_POINT('Ctrl Pts',(0.777263862165306,-2.25647828649788,
8.35220541029103));
#12023=CARTESIAN_POINT('Ctrl Pts',(0.764515912500924,-2.24860576017211,
8.38771594041925));
#12024=CARTESIAN_POINT('Ctrl Pts',(0.757692854619132,-2.24378973207509,
8.40584390296175));
#12025=CARTESIAN_POINT('Ctrl Pts',(0.749880792752036,-2.23311016839464,
8.42116977302821));
#12026=CARTESIAN_POINT('Ctrl Pts',(0.748053813348503,-2.23026329396527,
8.42439613938683));
#12027=CARTESIAN_POINT('Ctrl Pts',(0.74536508490224,-2.22489909228887,8.42792153395599));
#12028=CARTESIAN_POINT('Ctrl Pts',(0.74440239044637,-2.22270189648639,8.42889596208619));
#12029=CARTESIAN_POINT('Ctrl Pts',(0.742834762688225,-2.2183437876705,8.42963752815454));
#12030=CARTESIAN_POINT('Ctrl Pts',(0.742234963015787,-2.21635394379078,
8.42957119646972));
#12031=CARTESIAN_POINT('Ctrl Pts',(0.741219113742224,-2.21223036963063,
8.42860540961881));
#12032=CARTESIAN_POINT('Ctrl Pts',(0.740845869213951,-2.21021743019184,
8.42768512388005));
#12033=CARTESIAN_POINT('Ctrl Pts',(0.740183709016934,-2.20549798416793,
8.42469682244956));
#12034=CARTESIAN_POINT('Ctrl Pts',(0.740031560493762,-2.20294644611918,
8.42227427643572));
#12035=CARTESIAN_POINT('Ctrl Pts',(0.740001469953493,-2.20048719247971,
8.419426543521));
#12036=CARTESIAN_POINT('Ctrl Pts',(0.739999999999999,-2.20024249519991,
8.41913657657253));
#12037=CARTESIAN_POINT('Ctrl Pts',(0.739999999999999,-2.2,8.41884281581389));
#12038=CARTESIAN_POINT('',(0.740000088532922,-2.19989692748782,8.));
#12039=CARTESIAN_POINT('Origin',(0.8,-2.2,8.));
#12040=CARTESIAN_POINT('',(0.753574871202513,-2.16199069301438,8.27341677618955));
#12041=CARTESIAN_POINT('Ctrl Pts',(0.753574871223386,-2.16199069300718,
8.2734167761916));
#12042=CARTESIAN_POINT('Ctrl Pts',(0.754683939292676,-2.16063606089172,
8.25732450111787));
#12043=CARTESIAN_POINT('Ctrl Pts',(0.755525382712852,-2.15972125718946,
8.24070221271168));
#12044=CARTESIAN_POINT('Ctrl Pts',(0.757139618224984,-2.15797471815607,
8.17493064758107));
#12045=CARTESIAN_POINT('Ctrl Pts',(0.753939881287673,-2.16024262281511,
8.13023220048983));
#12046=CARTESIAN_POINT('Ctrl Pts',(0.744417566034987,-2.17594334474188,
8.05631746291443));
#12047=CARTESIAN_POINT('Ctrl Pts',(0.740253147200178,-2.18623233338143,
8.03133361374068));
#12048=CARTESIAN_POINT('Ctrl Pts',(0.740004341424627,-2.19919813034124,
8.00160163133619));
#12049=CARTESIAN_POINT('Ctrl Pts',(0.74000068880078,-2.19954750340221,8.00080090746578));
#12050=CARTESIAN_POINT('Ctrl Pts',(0.740000088532922,-2.19989692748782,
8.));
#12051=CARTESIAN_POINT('Ctrl Pts',(0.739999999999999,-2.2,8.41884281581389));
#12052=CARTESIAN_POINT('Ctrl Pts',(0.739999999999998,-2.19575754011241,
8.41370346363053));
#12053=CARTESIAN_POINT('Ctrl Pts',(0.740440387962112,-2.19219010800851,
8.40740207004508));
#12054=CARTESIAN_POINT('Ctrl Pts',(0.742244557849095,-2.18218933179936,
8.38643590161123));
#12055=CARTESIAN_POINT('Ctrl Pts',(0.74470820844627,-2.17604859945841,8.366170220377));
#12056=CARTESIAN_POINT('Ctrl Pts',(0.749610729583609,-2.16709782252209,
8.32084795754587));
#12057=CARTESIAN_POINT('Ctrl Pts',(0.751898667092447,-2.16403803348222,
8.29773804077552));
#12058=CARTESIAN_POINT('Ctrl Pts',(0.753574871223386,-2.16199069300717,
8.2734167761916));
#12059=CARTESIAN_POINT('Origin',(0.8,-2.2,11.));
#12060=CARTESIAN_POINT('Origin',(0.8,-2.2,8.));
#12061=CARTESIAN_POINT('',(0.8,-2.2,8.));
#12062=CARTESIAN_POINT('Origin',(0.8,-2.2,8.));
#12063=CARTESIAN_POINT('Origin',(0.8,-2.2,8.));
#12064=CARTESIAN_POINT('Ctrl Pts',(0.799999353205571,-2.14018795858917,
8.00474549279328));
#12065=CARTESIAN_POINT('Ctrl Pts',(0.799974799734663,-2.15448086801293,
8.18489286877592));
#12066=CARTESIAN_POINT('Ctrl Pts',(0.674665007466417,-2.18310389914977,
8.54360793631645));
#12067=CARTESIAN_POINT('Ctrl Pts',(0.189057319427946,-2.22621797906703,
8.84931316013818));
#12068=CARTESIAN_POINT('Ctrl Pts',(-0.382526459311769,-2.26949883233014,
8.78512361823764));
#12069=CARTESIAN_POINT('Ctrl Pts',(-0.807840639236961,-2.31455899583364,
8.36128354752488));
#12070=CARTESIAN_POINT('Ctrl Pts',(-0.841884630553248,-2.34849059789531,
7.90616153590567));
#12071=CARTESIAN_POINT('Ctrl Pts',(-0.706633312481697,-2.3776482221266,
7.56417102566761));
#12072=CARTESIAN_POINT('Ctrl Pts',(-0.524797421299121,-2.40036397277687,
7.33517763260607));
#12073=CARTESIAN_POINT('Ctrl Pts',(-0.184623097405697,-2.42964203470304,
7.17129916558269));
#12074=CARTESIAN_POINT('Ctrl Pts',(0.193484153574259,-2.4589910981866,7.17122122775637));
#12075=CARTESIAN_POINT('Ctrl Pts',(0.53519122257586,-2.48841027946974,7.33563982396839));
#12076=CARTESIAN_POINT('Ctrl Pts',(0.772150285550503,-2.51789845810207,
7.63264106317873));
#12077=CARTESIAN_POINT('Ctrl Pts',(0.857109363647141,-2.54745448449862,
8.00408762003218));
#12078=CARTESIAN_POINT('Ctrl Pts',(0.772052203859602,-2.5770771143395,8.37600483173473));
#12079=CARTESIAN_POINT('Ctrl Pts',(0.507269008134946,-2.61006365580992,
8.70902087610833));
#12080=CARTESIAN_POINT('Ctrl Pts',(0.184121132841334,-2.63651910824196,
8.83624322508014));
#12081=CARTESIAN_POINT('Ctrl Pts',(-0.066489483803979,-2.65639505342702,
8.83575881359142));
#12082=CARTESIAN_POINT('Ctrl Pts',(-0.272993262404685,-2.67296969383809,
8.80486180272118));
#12083=CARTESIAN_POINT('Ctrl Pts',(-0.542963798600168,-2.69620569938568,
8.6749478571166));
#12084=CARTESIAN_POINT('Ctrl Pts',(-0.783400610994973,-2.72613969346878,
8.3735180635455));
#12085=CARTESIAN_POINT('Ctrl Pts',(-0.884539863210645,-2.76112964475965,
7.93383176138089));
#12086=CARTESIAN_POINT('Ctrl Pts',(-0.709496036003296,-2.80121083689286,
7.43066574821048));
#12087=CARTESIAN_POINT('Ctrl Pts',(-0.200096069822599,-2.84642092016874,
7.11042023888795));
#12088=CARTESIAN_POINT('Ctrl Pts',(0.398680163779428,-2.89174303462223,
7.17762409038781));
#12089=CARTESIAN_POINT('Ctrl Pts',(0.826194257186495,-2.93717015873569,
7.60494403903258));
#12090=CARTESIAN_POINT('Ctrl Pts',(0.883028763967666,-2.97510749619044,
8.10591734828594));
#12091=CARTESIAN_POINT('Ctrl Pts',(0.733685094600885,-3.00550240345549,
8.46374186218363));
#12092=CARTESIAN_POINT('Ctrl Pts',(0.518762431301621,-3.03085542203816,
8.70482943573385));
#12093=CARTESIAN_POINT('Ctrl Pts',(0.194479876070813,-3.05877306117867,
8.86101946641206));
#12094=CARTESIAN_POINT('Ctrl Pts',(-0.198398854087579,-3.08926279897463,
8.86116295997746));
#12095=CARTESIAN_POINT('Ctrl Pts',(-0.552866770740287,-3.11978430147565,
8.69045288806385));
#12096=CARTESIAN_POINT('Ctrl Pts',(-0.798459570530803,-3.15033499607393,
8.38276097552609));
#12097=CARTESIAN_POINT('Ctrl Pts',(-0.886189886223361,-3.18091257250085,
7.9985222617957));
#12098=CARTESIAN_POINT('Ctrl Pts',(-0.805754444707439,-3.20896404488721,
7.64600910454789));
#12099=CARTESIAN_POINT('Ctrl Pts',(-0.617356025266483,-3.23448146889928,
7.38101130632405));
#12100=CARTESIAN_POINT('Ctrl Pts',(-0.299249903140631,-3.2651162608211,
7.15427322620025));
#12101=CARTESIAN_POINT('Ctrl Pts',(0.20669102063405,-3.30343842772452,7.09641469177514));
#12102=CARTESIAN_POINT('Ctrl Pts',(0.72520383869486,-3.34944736574065,7.4225450742071));
#12103=CARTESIAN_POINT('Ctrl Pts',(0.859802571238952,-3.38014846116659,
7.80703861326121));
#12104=CARTESIAN_POINT('Ctrl Pts',(0.859828918911975,-3.39548580458109,
8.00035000220606));
#12105=CARTESIAN_POINT('Ctrl Pts',(0.782047395351802,-2.14018795858917,
8.00474304600285));
#12106=CARTESIAN_POINT('Ctrl Pts',(0.782023383332822,-2.15416568148035,
8.18091782094919));
#12107=CARTESIAN_POINT('Ctrl Pts',(0.659521780500366,-2.18214688322478,
8.53162368091412));
#12108=CARTESIAN_POINT('Ctrl Pts',(0.18464317703468,-2.22430909576203,8.83062018723366));
#12109=CARTESIAN_POINT('Ctrl Pts',(-0.374447713497299,-2.26664059058254,
8.76785144918027));
#12110=CARTESIAN_POINT('Ctrl Pts',(-0.790610270786435,-2.31072617143467,
8.35318712238713));
#12111=CARTESIAN_POINT('Ctrl Pts',(-0.823965551575852,-2.34393500774394,
7.90772402533263));
#12112=CARTESIAN_POINT('Ctrl Pts',(-0.69154722527925,-2.37248233285328,
7.57288615600467));
#12113=CARTESIAN_POINT('Ctrl Pts',(-0.513499356518822,-2.3947239401174,
7.34864384720008));
#12114=CARTESIAN_POINT('Ctrl Pts',(-0.18028811648245,-2.4234026384316,7.18809946898689));
#12115=CARTESIAN_POINT('Ctrl Pts',(0.190198277819923,-2.45215741125776,
7.18800542247321));
#12116=CARTESIAN_POINT('Ctrl Pts',(0.525149537887764,-2.48099201036255,
7.34914925604369));
#12117=CARTESIAN_POINT('Ctrl Pts',(0.757517539664766,-2.50990501139262,
7.64036832969054));
#12118=CARTESIAN_POINT('Ctrl Pts',(0.840880626162148,-2.53889479412451,
8.00473123017728));
#12119=CARTESIAN_POINT('Ctrl Pts',(0.757422383748918,-2.56796498202542,
8.36973245506803));
#12120=CARTESIAN_POINT('Ctrl Pts',(0.497481478898117,-2.60034773025975,
8.69669786914853));
#12121=CARTESIAN_POINT('Ctrl Pts',(0.180051704651674,-2.62633437324586,
8.82170336201811));
#12122=CARTESIAN_POINT('Ctrl Pts',(-0.0662397268939709,-2.64586682880387,
8.8212287792569));
#12123=CARTESIAN_POINT('Ctrl Pts',(-0.269218207817606,-2.66215808538477,
8.79086083019633));
#12124=CARTESIAN_POINT('Ctrl Pts',(-0.534658210265181,-2.68500042855823,
8.66314528058294));
#12125=CARTESIAN_POINT('Ctrl Pts',(-0.77121061187554,-2.71444724443111,
8.36662469936537));
#12126=CARTESIAN_POINT('Ctrl Pts',(-0.870785710837989,-2.74888478105817,
7.93385634133438));
#12127=CARTESIAN_POINT('Ctrl Pts',(-0.698451578107866,-2.78835482764175,
7.43825459451075));
#12128=CARTESIAN_POINT('Ctrl Pts',(-0.196333892591823,-2.83291723989608,
7.12247712438595));
#12129=CARTESIAN_POINT('Ctrl Pts',(0.394483807013738,-2.87762888342211,
7.18869373683052));
#12130=CARTESIAN_POINT('Ctrl Pts',(0.81676492629728,-2.92248617467578,7.61064729804906));
#12131=CARTESIAN_POINT('Ctrl Pts',(0.87303850287666,-2.95998625249499,8.10588405657973));
#12132=CARTESIAN_POINT('Ctrl Pts',(0.725307987087691,-2.99005251598402,
8.45988987866063));
#12133=CARTESIAN_POINT('Ctrl Pts',(0.512589152625104,-3.0151452729584,8.69852906415756));
#12134=CARTESIAN_POINT('Ctrl Pts',(0.191449002788501,-3.04278955011802,
8.85323712338039));
#12135=CARTESIAN_POINT('Ctrl Pts',(-0.197922943695345,-3.07300561720271,
8.85341423236731));
#12136=CARTESIAN_POINT('Ctrl Pts',(-0.549461136454415,-3.10326898677065,
8.68414590340907));
#12137=CARTESIAN_POINT('Ctrl Pts',(-0.793229818870514,-3.13358792502119,
8.37879861499031));
#12138=CARTESIAN_POINT('Ctrl Pts',(-0.880383072820295,-3.1639499541908,
7.99721589789444));
#12139=CARTESIAN_POINT('Ctrl Pts',(-0.800475324765631,-3.1918254698827,
7.64687170048445));
#12140=CARTESIAN_POINT('Ctrl Pts',(-0.61312934238898,-3.21719954694791,
7.38332949897577));
#12141=CARTESIAN_POINT('Ctrl Pts',(-0.296622142271461,-3.24767997051828,
7.15770725112751));
#12142=CARTESIAN_POINT('Ctrl Pts',(0.207147409687023,-3.28583242893591,
7.10000791688759));
#12143=CARTESIAN_POINT('Ctrl Pts',(0.724104113244679,-3.33169443325757,
7.42503466252389));
#12144=CARTESIAN_POINT('Ctrl Pts',(0.858447915360046,-3.36232685262669,
7.80874538280109));
#12145=CARTESIAN_POINT('Ctrl Pts',(0.858474223399892,-3.37764112502309,
8.00176598536707));
#12146=CARTESIAN_POINT('Ctrl Pts',(0.74625274599145,-2.15732833022565,8.00337824864829));
#12147=CARTESIAN_POINT('Ctrl Pts',(0.746229817884691,-2.17067509306803,
8.17160042319879));
#12148=CARTESIAN_POINT('Ctrl Pts',(0.629314000947051,-2.19736550953753,
8.50610935856775));
#12149=CARTESIAN_POINT('Ctrl Pts',(0.176611094607005,-2.23755733973025,
8.79107825953155));
#12150=CARTESIAN_POINT('Ctrl Pts',(-0.355910946191055,-2.27787674797685,
8.73120669874899));
#12151=CARTESIAN_POINT('Ctrl Pts',(-0.752030415880074,-2.31984419599776,
8.33643709393526));
#12152=CARTESIAN_POINT('Ctrl Pts',(-0.783731715249715,-2.35144232472123,
7.91257415253098));
#12153=CARTESIAN_POINT('Ctrl Pts',(-0.657760402987585,-2.37859990065862,
7.59404159903955));
#12154=CARTESIAN_POINT('Ctrl Pts',(-0.488391328153346,-2.3997571052949,
7.38074179934443));
#12155=CARTESIAN_POINT('Ctrl Pts',(-0.17146818986477,-2.42703420947409,
7.22805123116321));
#12156=CARTESIAN_POINT('Ctrl Pts',(0.180899194564967,-2.45438379948815,
7.22796563928441));
#12157=CARTESIAN_POINT('Ctrl Pts',(0.499476525914112,-2.48181004852974,
7.38123478608588));
#12158=CARTESIAN_POINT('Ctrl Pts',(0.720509655667483,-2.50931350242048,
7.65824455912636));
#12159=CARTESIAN_POINT('Ctrl Pts',(0.799820849374384,-2.53689527427906,
8.00488898306531));
#12160=CARTESIAN_POINT('Ctrl Pts',(0.720413518964486,-2.56455811211287,
8.35221369057467));
#12161=CARTESIAN_POINT('Ctrl Pts',(0.472996082608528,-2.59538372533697,
8.66344434480147));
#12162=CARTESIAN_POINT('Ctrl Pts',(0.170739321333303,-2.62012995691034,
8.78249789645164));
#12163=CARTESIAN_POINT('Ctrl Pts',(-0.0638674325015451,-2.63873618276797,
8.78204801163947));
#12164=CARTESIAN_POINT('Ctrl Pts',(-0.257241904787735,-2.65425698108223,
8.75311696166082));
#12165=CARTESIAN_POINT('Ctrl Pts',(-0.510220632940824,-2.67602856460628,
8.63141433807984));
#12166=CARTESIAN_POINT('Ctrl Pts',(-0.735784166111144,-2.70410650625065,
8.34869879134964));
#12167=CARTESIAN_POINT('Ctrl Pts',(-0.830811311210507,-2.73696323384205,
7.9358300220051));
#12168=CARTESIAN_POINT('Ctrl Pts',(-0.666338844974052,-2.77465593116664,
7.46259060542153));
#12169=CARTESIAN_POINT('Ctrl Pts',(-0.186452486819304,-2.81725520701278,
7.16066959619675));
#12170=CARTESIAN_POINT('Ctrl Pts',(0.378959513489126,-2.86004954464569,
7.2239233219175));
#12171=CARTESIAN_POINT('Ctrl Pts',(0.783699385156277,-2.90303928187437,
7.62816364103489));
#12172=CARTESIAN_POINT('Ctrl Pts',(0.837802742196778,-2.9390268509025,8.10336709497288));
#12173=CARTESIAN_POINT('Ctrl Pts',(0.695903933635387,-2.96791382473259,
8.44346809432988));
#12174=CARTESIAN_POINT('Ctrl Pts',(0.491405830641922,-2.99204008047502,
8.67290813935407));
#12175=CARTESIAN_POINT('Ctrl Pts',(0.18237238112984,-3.01864752247096,8.82183051955883));
#12176=CARTESIAN_POINT('Ctrl Pts',(-0.192742934390733,-3.04775885609569,
8.82204356332466));
#12177=CARTESIAN_POINT('Ctrl Pts',(-0.531846282469671,-3.07695455750375,
8.65882083669825));
#12178=CARTESIAN_POINT('Ctrl Pts',(-0.767277470964291,-3.1062336310193,
8.36398870428271));
#12179=CARTESIAN_POINT('Ctrl Pts',(-0.851599932176543,-3.1355956353591,
7.99504782175763));
#12180=CARTESIAN_POINT('Ctrl Pts',(-0.774285320211519,-3.16258542373216,
7.65586242334073));
#12181=CARTESIAN_POINT('Ctrl Pts',(-0.592726533508006,-3.18718054137099,
7.40042073906037));
#12182=CARTESIAN_POINT('Ctrl Pts',(-0.285687289089679,-3.2167534027861,
7.18150928308508));
#12183=CARTESIAN_POINT('Ctrl Pts',(0.203822077518427,-3.2538348995878,7.12528061883726));
#12184=CARTESIAN_POINT('Ctrl Pts',(0.707318122939241,-3.2984956193622,7.44157309236475));
#12185=CARTESIAN_POINT('Ctrl Pts',(0.838602160088046,-3.32839609386495,
7.81596220818301));
#12186=CARTESIAN_POINT('Ctrl Pts',(0.838627855643513,-3.34335383066725,
8.0044890474524));
#12187=CARTESIAN_POINT('Ctrl Pts',(0.733109166050823,-2.21520789437687,
7.99878428726588));
#12188=CARTESIAN_POINT('Ctrl Pts',(0.733086651152081,-2.22831412321213,
8.16397477883759));
#12189=CARTESIAN_POINT('Ctrl Pts',(0.61820806476396,-2.25448891667089,8.4918749804416));
#12190=CARTESIAN_POINT('Ctrl Pts',(0.175997071981037,-2.2937344485149,8.76979482863797));
#12191=CARTESIAN_POINT('Ctrl Pts',(-0.341851058364153,-2.33295097190823,
8.71124005417684));
#12192=CARTESIAN_POINT('Ctrl Pts',(-0.725322381060742,-2.37361034528651,
8.3285616317421));
#12193=CARTESIAN_POINT('Ctrl Pts',(-0.755620395377764,-2.40410249010971,
7.91958143791062));
#12194=CARTESIAN_POINT('Ctrl Pts',(-0.634368791517699,-2.43024050309635,
7.61303100221757));
#12195=CARTESIAN_POINT('Ctrl Pts',(-0.471556266419422,-2.45057518839065,
7.40809066379694));
#12196=CARTESIAN_POINT('Ctrl Pts',(-0.167691580481213,-2.4767255191272,
7.26180006781177));
#12197=CARTESIAN_POINT('Ctrl Pts',(0.169354507378634,-2.50288963142343,
7.26180070426125));
#12198=CARTESIAN_POINT('Ctrl Pts',(0.473364185136383,-2.52906730718321,
7.40815784881158));
#12199=CARTESIAN_POINT('Ctrl Pts',(0.683803616304868,-2.555262600058,7.67201422540797));
#12200=CARTESIAN_POINT('Ctrl Pts',(0.759102306253096,-2.58147909308525,
8.00147874603806));
#12201=CARTESIAN_POINT('Ctrl Pts',(0.683721893443959,-2.60771728231028,
8.33088235794537));
#12202=CARTESIAN_POINT('Ctrl Pts',(0.449432489049715,-2.63690187004837,
8.62546727981126));
#12203=CARTESIAN_POINT('Ctrl Pts',(0.163874330576686,-2.66027910711593,
8.73783282899925));
#12204=CARTESIAN_POINT('Ctrl Pts',(-0.0574129106102927,-2.6778300800841,
8.73740397568539));
#12205=CARTESIAN_POINT('Ctrl Pts',(-0.239710347551256,-2.69246200371179,
8.71012676650314));
#12206=CARTESIAN_POINT('Ctrl Pts',(-0.47792311168767,-2.71296689041938,
8.59547666875305));
#12207=CARTESIAN_POINT('Ctrl Pts',(-0.689948244038352,-2.73936587099675,
8.32963733232912));
#12208=CARTESIAN_POINT('Ctrl Pts',(-0.779095823746774,-2.77021281732857,
7.94202402152301));
#12209=CARTESIAN_POINT('Ctrl Pts',(-0.62481378813293,-2.80554090335429,
7.49856445460143));
#12210=CARTESIAN_POINT('Ctrl Pts',(-0.175855711648067,-2.84539012232819,
7.21629185933956));
#12211=CARTESIAN_POINT('Ctrl Pts',(0.352109156831138,-2.88535475052917,
7.27549305282249));
#12212=CARTESIAN_POINT('Ctrl Pts',(0.72941562263406,-2.92544247381862,7.65250150966383));
#12213=CARTESIAN_POINT('Ctrl Pts',(0.779714856881808,-2.9589572593585,8.09504757135279));
#12214=CARTESIAN_POINT('Ctrl Pts',(0.647663516769697,-2.98583864019596,
8.41151349407204));
#12215=CARTESIAN_POINT('Ctrl Pts',(0.45745146394856,-3.00827891026592,8.62491004682719));
#12216=CARTESIAN_POINT('Ctrl Pts',(0.170146416399821,-3.03301596259707,
8.7633430911453));
#12217=CARTESIAN_POINT('Ctrl Pts',(-0.178425509553831,-3.06006759257889,
8.76352533431625));
#12218=CARTESIAN_POINT('Ctrl Pts',(-0.493423394438939,-3.08718913671925,
8.61189555627018));
#12219=CARTESIAN_POINT('Ctrl Pts',(-0.712056882382278,-3.1143800682777,
8.33808617234675));
#12220=CARTESIAN_POINT('Ctrl Pts',(-0.790352964968391,-3.14164438601587,
7.99550913276558));
#12221=CARTESIAN_POINT('Ctrl Pts',(-0.718569670978983,-3.16670409444998,
7.68058308222211));
#12222=CARTESIAN_POINT('Ctrl Pts',(-0.549995050890336,-3.18954068246379,
7.44339985556457));
#12223=CARTESIAN_POINT('Ctrl Pts',(-0.264888955600131,-3.21700180066857,
7.2401273936459));
#12224=CARTESIAN_POINT('Ctrl Pts',(0.18973412922727,-3.25143927114534,7.18784224870088));
#12225=CARTESIAN_POINT('Ctrl Pts',(0.657612957996916,-3.29294170706199,
7.48173687430083));
#12226=CARTESIAN_POINT('Ctrl Pts',(0.779716152438242,-3.3207351361234,7.8297224617271));
#12227=CARTESIAN_POINT('Ctrl Pts',(0.779740067663557,-3.33465651822015,
8.00518711922511));
#12228=CARTESIAN_POINT('Ctrl Pts',(0.770174713816319,-2.26178036861328,
7.99509427477235));
#12229=CARTESIAN_POINT('Ctrl Pts',(0.770151085712947,-2.27553460900681,
8.16845228342319));
#12230=CARTESIAN_POINT('Ctrl Pts',(0.649526282375535,-2.30298809044055,
8.51236935836145));
#12231=CARTESIAN_POINT('Ctrl Pts',(0.187191988159535,-2.34399875981116,
8.80253374467715));
#12232=CARTESIAN_POINT('Ctrl Pts',(-0.352122720593585,-2.38484196589621,
8.74127014025205));
#12233=CARTESIAN_POINT('Ctrl Pts',(-0.74981389952082,-2.42703190005934,
8.34386831568528));
#12234=CARTESIAN_POINT('Ctrl Pts',(-0.780810988575083,-2.45854730667668,
7.92110588453579));
#12235=CARTESIAN_POINT('Ctrl Pts',(-0.655782055676547,-2.48549706819932,
7.60504883404085));
#12236=CARTESIAN_POINT('Ctrl Pts',(-0.488152229522925,-2.50642282845949,
7.39416068503242));
#12237=CARTESIAN_POINT('Ctrl Pts',(-0.17617063943151,-2.53326677800351,
7.24407668777915));
#12238=CARTESIAN_POINT('Ctrl Pts',(0.168881610443051,-2.56004874071718,
7.24418064291107));
#12239=CARTESIAN_POINT('Ctrl Pts',(0.479230965544757,-2.58677333437478,
7.39370222330362));
#12240=CARTESIAN_POINT('Ctrl Pts',(0.693414173896507,-2.61344224384572,
7.66242541074539));
#12241=CARTESIAN_POINT('Ctrl Pts',(0.769764263667122,-2.64005723004352,
7.99696854387048));
#12242=CARTESIAN_POINT('Ctrl Pts',(0.693335561872293,-2.66662311576071,
8.3304793629683));
#12243=CARTESIAN_POINT('Ctrl Pts',(0.456681051153885,-2.69608560261765,
8.62783081941731));
#12244=CARTESIAN_POINT('Ctrl Pts',(0.16924819913035,-2.7196091352219,8.7407546542504));
#12245=CARTESIAN_POINT('Ctrl Pts',(-0.0529090347140539,-2.73722886357395,
8.74031178383068));
#12246=CARTESIAN_POINT('Ctrl Pts',(-0.23576095072381,-2.75190456253053,
8.71294659686804));
#12247=CARTESIAN_POINT('Ctrl Pts',(-0.474181034064131,-2.77242751342201,
8.59809544867928));
#12248=CARTESIAN_POINT('Ctrl Pts',(-0.685755228804926,-2.79877927012082,
8.33265644851143));
#12249=CARTESIAN_POINT('Ctrl Pts',(-0.774362457417276,-2.82948181440773,
7.94678514096296));
#12250=CARTESIAN_POINT('Ctrl Pts',(-0.62102565384786,-2.86451451341815,
7.5070541202394));
#12251=CARTESIAN_POINT('Ctrl Pts',(-0.177411403127165,-2.90386624093258,
7.22859186809493));
#12252=CARTESIAN_POINT('Ctrl Pts',(0.341805275122635,-2.94316555019382,
7.28718194578695));
#12253=CARTESIAN_POINT('Ctrl Pts',(0.711089238372315,-2.98242344371321,
7.65669609347703));
#12254=CARTESIAN_POINT('Ctrl Pts',(0.759874955551073,-3.01511362277788,
8.08842693995537));
#12255=CARTESIAN_POINT('Ctrl Pts',(0.631394082076154,-3.04125498629743,
8.39617192670839));
#12256=CARTESIAN_POINT('Ctrl Pts',(0.446727094145398,-3.06303575794805,
8.60328587127767));
#12257=CARTESIAN_POINT('Ctrl Pts',(0.168447547207533,-3.08698931162158,
8.73726657609774));
#12258=CARTESIAN_POINT('Ctrl Pts',(-0.168284740868862,-3.11312097384991,
8.73735081104941));
#12259=CARTESIAN_POINT('Ctrl Pts',(-0.471770516529958,-3.13925157733386,
8.5911521718779));
#12260=CARTESIAN_POINT('Ctrl Pts',(-0.681876290605352,-3.16538945158193,
8.32788280407561));
#12261=CARTESIAN_POINT('Ctrl Pts',(-0.75687043959184,-3.19153241519703,
7.99933013384828));
#12262=CARTESIAN_POINT('Ctrl Pts',(-0.688110617431308,-3.21550770668684,
7.69802709281149));
#12263=CARTESIAN_POINT('Ctrl Pts',(-0.527102437271904,-3.23731354435981,
7.47155051476055));
#12264=CARTESIAN_POINT('Ctrl Pts',(-0.255247811551174,-3.26349398274227,
7.27779274208));
#12265=CARTESIAN_POINT('Ctrl Pts',(0.177152842785472,-3.29623830622227,
7.22824975845271));
#12266=CARTESIAN_POINT('Ctrl Pts',(0.620660945134379,-3.33559389149627,
7.50721088384051));
#12267=CARTESIAN_POINT('Ctrl Pts',(0.735928860988268,-3.36185737845845,
7.8361523880049));
#12268=CARTESIAN_POINT('Ctrl Pts',(0.735951464222257,-3.37501503233047,
8.0019910392312));
#12269=CARTESIAN_POINT('Ctrl Pts',(0.829757440060419,-2.26160662142564,
7.99511618081194));
#12270=CARTESIAN_POINT('Ctrl Pts',(0.829732011685375,-2.27640882444931,
8.18168267713667));
#12271=CARTESIAN_POINT('Ctrl Pts',(0.699816007409573,-2.30598791214416,
8.55221812941387));
#12272=CARTESIAN_POINT('Ctrl Pts',(0.201827204414,-2.35015821050548,8.86470616099201));
#12273=CARTESIAN_POINT('Ctrl Pts',(-0.379023488117868,-2.39415086067652,
8.798733952075));
#12274=CARTESIAN_POINT('Ctrl Pts',(-0.807163231352076,-2.43957549257121,
8.37081904005922));
#12275=CARTESIAN_POINT('Ctrl Pts',(-0.840454824876188,-2.47348909800905,
7.91591570873383));
#12276=CARTESIAN_POINT('Ctrl Pts',(-0.705987307445184,-2.50247231543482,
7.57601597628261));
#12277=CARTESIAN_POINT('Ctrl Pts',(-0.525755857322679,-2.52497039347374,
7.34930933428415));
#12278=CARTESIAN_POINT('Ctrl Pts',(-0.190564709372351,-2.55381055956905,
7.18809737406272));
#12279=CARTESIAN_POINT('Ctrl Pts',(0.179868561363044,-2.58256433966825,
7.18824648518451));
#12280=CARTESIAN_POINT('Ctrl Pts',(0.512742434807326,-2.61123160277901,
7.3486676190774));
#12281=CARTESIAN_POINT('Ctrl Pts',(0.742233225896921,-2.63981211857978,
7.63666503815448));
#12282=CARTESIAN_POINT('Ctrl Pts',(0.823917156000059,-2.66830610941488,
7.99481197794227));
#12283=CARTESIAN_POINT('Ctrl Pts',(0.742148744255773,-2.69671317878052,
8.35141437252788));
#12284=CARTESIAN_POINT('Ctrl Pts',(0.489351482775192,-2.72818096959852,
8.66894559809407));
#12285=CARTESIAN_POINT('Ctrl Pts',(0.182823382372039,-2.75326575186073,
8.78927701682514));
#12286=CARTESIAN_POINT('Ctrl Pts',(-0.0537740200675628,-2.77203170033953,
8.78879919988707));
#12287=CARTESIAN_POINT('Ctrl Pts',(-0.248418830469036,-2.78765413923565,
8.75966578777999));
#12288=CARTESIAN_POINT('Ctrl Pts',(-0.501950393695151,-2.80948215695733,
8.6374786190774));
#12289=CARTESIAN_POINT('Ctrl Pts',(-0.726531624311689,-2.83746139454138,
8.35561440545181));
#12290=CARTESIAN_POINT('Ctrl Pts',(-0.820370674170875,-2.8700064123799,
7.94658577453689));
#12291=CARTESIAN_POINT('Ctrl Pts',(-0.657979802162612,-2.90706403447766,
7.48157410220611));
#12292=CARTESIAN_POINT('Ctrl Pts',(-0.189982629638962,-2.9485699800761,
7.18813916684599));
#12293=CARTESIAN_POINT('Ctrl Pts',(0.355914283630534,-2.98989709841734,
7.2500307715348));
#12294=CARTESIAN_POINT('Ctrl Pts',(0.742747929313828,-3.03104923641469,
7.63753899362132));
#12295=CARTESIAN_POINT('Ctrl Pts',(0.793447036700908,-3.06520022873892,
8.08855426316809));
#12296=CARTESIAN_POINT('Ctrl Pts',(0.659538652208142,-3.09243881334936,
8.40914673502315));
#12297=CARTESIAN_POINT('Ctrl Pts',(0.4674503800378,-3.11509225286223,8.62451838266328));
#12298=CARTESIAN_POINT('Ctrl Pts',(0.178601860616001,-3.13995544254992,
8.76348553257992));
#12299=CARTESIAN_POINT('Ctrl Pts',(-0.169989036987309,-3.16700866084923,
8.76347040877462));
#12300=CARTESIAN_POINT('Ctrl Pts',(-0.483342670519688,-3.19399683667518,
8.61240741646133));
#12301=CARTESIAN_POINT('Ctrl Pts',(-0.699654697307745,-3.22091820440651,
8.34118976706614));
#12302=CARTESIAN_POINT('Ctrl Pts',(-0.776595267516835,-3.24777858249128,
8.00364839053361));
#12303=CARTESIAN_POINT('Ctrl Pts',(-0.706051258169142,-3.27234450691577,
7.69497590786256));
#12304=CARTESIAN_POINT('Ctrl Pts',(-0.541450566177014,-3.29463393432445,
7.46352675713963));
#12305=CARTESIAN_POINT('Ctrl Pts',(-0.264114921152119,-3.32133928901001,
7.2659407429079));
#12306=CARTESIAN_POINT('Ctrl Pts',(0.175653891720555,-3.35464280170236,
7.21584666351496));
#12307=CARTESIAN_POINT('Ctrl Pts',(0.624550632429727,-3.39449891025175,
7.49865340549804));
#12308=CARTESIAN_POINT('Ctrl Pts',(0.740598756530013,-3.42098439776615,
7.83036302208991));
#12309=CARTESIAN_POINT('Ctrl Pts',(0.740621508425407,-3.43422858948904,
7.99729239363825));
#12310=CARTESIAN_POINT('Ctrl Pts',(0.86707857137678,-2.21527214004116,7.99879744958048));
#12311=CARTESIAN_POINT('Ctrl Pts',(0.867052009824273,-2.23073398108044,
8.19367800248297));
#12312=CARTESIAN_POINT('Ctrl Pts',(0.731286147591186,-2.26168598382591,
8.58142473244992));
#12313=CARTESIAN_POINT('Ctrl Pts',(0.208931008692675,-2.30803255060304,
8.90953225625817));
#12314=CARTESIAN_POINT('Ctrl Pts',(-0.402279795131404,-2.35432607147985,
8.84040847995338));
#12315=CARTESIAN_POINT('Ctrl Pts',(-0.85419214733997,-2.40225297340794,
8.38916286237217));
#12316=CARTESIAN_POINT('Ctrl Pts',(-0.88965534661522,-2.4381319659943,7.90795747806708));
#12317=CARTESIAN_POINT('Ctrl Pts',(-0.747191693894078,-2.4688399396954,
7.54781745305364));
#12318=CARTESIAN_POINT('Ctrl Pts',(-0.556071742805826,-2.49270484793502,
7.30732995556476));
#12319=CARTESIAN_POINT('Ctrl Pts',(-0.200048697492744,-2.52334022091847,
7.13602410911045));
#12320=CARTESIAN_POINT('Ctrl Pts',(0.194018639288425,-2.55393045636901,
7.13611701708511));
#12321=CARTESIAN_POINT('Ctrl Pts',(0.548640567302356,-2.58446945367359,
7.3069515339409));
#12322=CARTESIAN_POINT('Ctrl Pts',(0.793472676065515,-2.61495596112549,
7.61410479143909));
#12323=CARTESIAN_POINT('Ctrl Pts',(0.880764541866717,-2.64538780695502,
7.99658056852376));
#12324=CARTESIAN_POINT('Ctrl Pts',(0.793387375209798,-2.67576077225686,
8.37786647565061));
#12325=CARTESIAN_POINT('Ctrl Pts',(0.522853213263504,-2.70944332490509,
8.71777142840022));
#12326=CARTESIAN_POINT('Ctrl Pts',(0.194405270094262,-2.73632442536312,
8.8467788012416));
#12327=CARTESIAN_POINT('Ctrl Pts',(-0.0593225760385914,-2.75644899867342,
8.84627081900103));
#12328=CARTESIAN_POINT('Ctrl Pts',(-0.26811681268387,-2.77320721193081,
8.81502223178674));
#12329=CARTESIAN_POINT('Ctrl Pts',(-0.540247683922515,-2.79663560807698,
8.68390627847152));
#12330=CARTESIAN_POINT('Ctrl Pts',(-0.78149729335789,-2.82668832932834,
8.38117208069794));
#12331=CARTESIAN_POINT('Ctrl Pts',(-0.882393815086409,-2.86166862077938,
7.94154547407333));
#12332=CARTESIAN_POINT('Ctrl Pts',(-0.707795934997192,-2.90152720543561,
7.44135040812137));
#12333=CARTESIAN_POINT('Ctrl Pts',(-0.204107195235052,-2.94620036140782,
7.12545965332791));
#12334=CARTESIAN_POINT('Ctrl Pts',(0.383742278004164,-2.99070111215732,
7.19206409213777));
#12335=CARTESIAN_POINT('Ctrl Pts',(0.800421419505439,-3.03502472007537,
7.60944125035824));
#12336=CARTESIAN_POINT('Ctrl Pts',(0.855035679658814,-3.0718098054969,8.0952640245661));
#12337=CARTESIAN_POINT('Ctrl Pts',(0.710808338022248,-3.10114549328222,
8.44055327044642));
#12338=CARTESIAN_POINT('Ctrl Pts',(0.503947744187646,-3.12554011221735,
8.67248640703811));
#12339=CARTESIAN_POINT('Ctrl Pts',(0.192957910284852,-3.1523069335416,8.82209610703405));
#12340=CARTESIAN_POINT('Ctrl Pts',(-0.182227420528306,-3.18142312386516,
8.82206702034478));
#12341=CARTESIAN_POINT('Ctrl Pts',(-0.519316204583526,-3.2104536203229,
8.65954066193778));
#12342=CARTESIAN_POINT('Ctrl Pts',(-0.751885348749804,-3.23939925187631,
8.36790792232583));
#12343=CARTESIAN_POINT('Ctrl Pts',(-0.834531785156997,-3.26825784301778,
8.00521528728933));
#12344=CARTESIAN_POINT('Ctrl Pts',(-0.758762890055745,-3.29463265406983,
7.67379560957547));
#12345=CARTESIAN_POINT('Ctrl Pts',(-0.582145976295626,-3.31854651420027,
7.42547621523144));
#12346=CARTESIAN_POINT('Ctrl Pts',(-0.284767910361057,-3.3471788646333,
7.21363048066223));
#12347=CARTESIAN_POINT('Ctrl Pts',(0.186219878216593,-3.38284229741198,
7.16011863942536));
#12348=CARTESIAN_POINT('Ctrl Pts',(0.666069785790777,-3.42545036202905,
7.46260932525095));
#12349=CARTESIAN_POINT('Ctrl Pts',(0.789761191020466,-3.45371486538175,
7.8167106365808));
#12350=CARTESIAN_POINT('Ctrl Pts',(0.789785439415121,-3.46783018993909,
7.99461973868823));
#12351=CARTESIAN_POINT('Ctrl Pts',(0.853613778380816,-2.15732131048097,
8.00339343853682));
#12352=CARTESIAN_POINT('Ctrl Pts',(0.853587606604479,-2.17255625750892,
8.19541422653387));
#12353=CARTESIAN_POINT('Ctrl Pts',(0.71993526562251,-2.20307513036369,8.57788731388851));
#12354=CARTESIAN_POINT('Ctrl Pts',(0.202998077757662,-2.24895826646226,
8.90308049625081));
#12355=CARTESIAN_POINT('Ctrl Pts',(-0.404350822674032,-2.29494956399607,
8.83473441415818));
#12356=CARTESIAN_POINT('Ctrl Pts',(-0.855322089232105,-2.34274179079025,
8.38500627260658));
#12357=CARTESIAN_POINT('Ctrl Pts',(-0.891159898667268,-2.3786574478564,
7.90325459408232));
#12358=CARTESIAN_POINT('Ctrl Pts',(-0.748187122836472,-2.40947785315607,
7.54177066796142));
#12359=CARTESIAN_POINT('Ctrl Pts',(-0.556127946781633,-2.43346472037247,
7.29998095570304));
#12360=CARTESIAN_POINT('Ctrl Pts',(-0.197400708727537,-2.46433665913889,
7.1272421567771));
#12361=CARTESIAN_POINT('Ctrl Pts',(0.200669460267103,-2.4952342052595,7.12723282118374));
#12362=CARTESIAN_POINT('Ctrl Pts',(0.559810871311599,-2.52615645882231,
7.30012245677509));
#12363=CARTESIAN_POINT('Ctrl Pts',(0.808408390951575,-2.55709970891155,
7.61183546841623));
#12364=CARTESIAN_POINT('Ctrl Pts',(0.897329380531666,-2.58806086349922,
8.00097004624504));
#12365=CARTESIAN_POINT('Ctrl Pts',(0.808306642551815,-2.61903782660728,
8.38987609029684));
#12366=CARTESIAN_POINT('Ctrl Pts',(0.531836448053288,-2.65346946876861,
8.73743082896215));
#12367=CARTESIAN_POINT('Ctrl Pts',(0.195204243964366,-2.68102443097052,
8.86982140892509));
#12368=CARTESIAN_POINT('Ctrl Pts',(-0.0654014761015361,-2.70169345944525,
8.8693080479456));
#12369=CARTESIAN_POINT('Ctrl Pts',(-0.28001061760865,-2.71891842965623,
8.83719397053499));
#12370=CARTESIAN_POINT('Ctrl Pts',(-0.56017691686546,-2.74303440031375,
8.70229225968454));
#12371=CARTESIAN_POINT('Ctrl Pts',(-0.809160087931685,-2.77404089873971,
8.39000815585855));
#12372=CARTESIAN_POINT('Ctrl Pts',(-0.913602970950101,-2.81021106185289,
7.93545491025926));
#12373=CARTESIAN_POINT('Ctrl Pts',(-0.732844719291178,-2.85153775103447,
7.41673989523743));
#12374=CARTESIAN_POINT('Ctrl Pts',(-0.209092138228919,-2.898005510644,7.08787736303838));
#12375=CARTESIAN_POINT('Ctrl Pts',(0.404314566935514,-2.94443832383181,
7.15706703724753));
#12376=CARTESIAN_POINT('Ctrl Pts',(0.840611098505371,-2.99082585871325,
7.59366406143764));
#12377=CARTESIAN_POINT('Ctrl Pts',(0.898167561855067,-3.0294358538606,8.10354953547171));
#12378=CARTESIAN_POINT('Ctrl Pts',(0.746510298453132,-3.06029121684836,
8.4667497767436));
#12379=CARTESIAN_POINT('Ctrl Pts',(0.528670012322939,-3.08598436655093,
8.71104238802412));
#12380=CARTESIAN_POINT('Ctrl Pts',(0.200651339320336,-3.11422060483273,
8.86892278377001));
#12381=CARTESIAN_POINT('Ctrl Pts',(-0.195786982033943,-3.14498685758523,
8.86896376428506));
#12382=CARTESIAN_POINT('Ctrl Pts',(-0.552599640454179,-3.17571518690325,
8.69700649395508));
#12383=CARTESIAN_POINT('Ctrl Pts',(-0.799192405052644,-3.20640067964169,
8.38789335444557));
#12384=CARTESIAN_POINT('Ctrl Pts',(-0.887002523210114,-3.23704301100247,
8.00282800313923));
#12385=CARTESIAN_POINT('Ctrl Pts',(-0.806491468029696,-3.2650882512832,
7.65042392555724));
#12386=CARTESIAN_POINT('Ctrl Pts',(-0.6184882410522,-3.29054770478482,7.38606022980516));
#12387=CARTESIAN_POINT('Ctrl Pts',(-0.301617462444111,-3.32105973226801,
7.16028129179456));
#12388=CARTESIAN_POINT('Ctrl Pts',(0.201027370363033,-3.3591287320595,7.10307029008688));
#12389=CARTESIAN_POINT('Ctrl Pts',(0.714123794960093,-3.40467760024813,
7.42624743346387));
#12390=CARTESIAN_POINT('Ctrl Pts',(0.846710623234168,-3.43496022264899,
7.80554292001516));
#12391=CARTESIAN_POINT('Ctrl Pts',(0.846736584716904,-3.45007275937647,
7.99602085262167));
#12392=CARTESIAN_POINT('Ctrl Pts',(0.817951311059339,-2.14018795858917,
8.00474793958371));
#12393=CARTESIAN_POINT('Ctrl Pts',(0.817926216049528,-2.15479610517542,
8.18886855474053));
#12394=CARTESIAN_POINT('Ctrl Pts',(0.689817303447149,-2.18405877779726,
8.55560183955968));
#12395=CARTESIAN_POINT('Ctrl Pts',(0.19347377106145,-2.22812384223798,8.86803409341903));
#12396=CARTESIAN_POINT('Ctrl Pts',(-0.390624346224737,-2.27235269475253,
8.80243528497531));
#12397=CARTESIAN_POINT('Ctrl Pts',(-0.825118707115923,-2.3183864962394,
8.36940838838631));
#12398=CARTESIAN_POINT('Ctrl Pts',(-0.859860802914712,-2.35303977428868,
7.9046020627869));
#12399=CARTESIAN_POINT('Ctrl Pts',(-0.721763577837354,-2.38281053702234,
7.55541942075108));
#12400=CARTESIAN_POINT('Ctrl Pts',(-0.536133762339803,-2.40599896833622,
7.32165570099066));
#12401=CARTESIAN_POINT('Ctrl Pts',(-0.18895749473576,-2.43587876194045,
7.15441590182363));
#12402=CARTESIAN_POINT('Ctrl Pts',(0.196802128379297,-2.46582051078235,
7.15434610219188));
#12403=CARTESIAN_POINT('Ctrl Pts',(0.545307786053435,-2.49582411881007,
7.32204685195694));
#12404=CARTESIAN_POINT('Ctrl Pts',(0.786887979130198,-2.52588746642215,
7.62486140910485));
#12405=CARTESIAN_POINT('Ctrl Pts',(0.873463361515396,-2.55600774488533,
8.00342516000178));
#12406=CARTESIAN_POINT('Ctrl Pts',(0.78679367211852,-2.58618568236755,8.38231958055917));
#12407=CARTESIAN_POINT('Ctrl Pts',(0.517143884962038,-2.61977459658829,
8.72142638757352));
#12408=CARTESIAN_POINT('Ctrl Pts',(0.188227088153933,-2.64670029064388,
8.85088945134281));
#12409=CARTESIAN_POINT('Ctrl Pts',(-0.0667518101348738,-2.6669222358181,
8.85039427757092));
#12410=CARTESIAN_POINT('Ctrl Pts',(-0.276825487921848,-2.68378301119882,
8.81896286031109));
#12411=CARTESIAN_POINT('Ctrl Pts',(-0.551354493616545,-2.7074097040812,
8.68683667774742));
#12412=CARTESIAN_POINT('Ctrl Pts',(-0.795733091743474,-2.73783532831967,
8.38043509041218));
#12413=CARTESIAN_POINT('Ctrl Pts',(-0.898456345943392,-2.77338063567163,
7.93373612144092));
#12414=CARTESIAN_POINT('Ctrl Pts',(-0.720680695041125,-2.81406632664805,
7.42293130178022));
#12415=CARTESIAN_POINT('Ctrl Pts',(-0.203901168868501,-2.85992243385813,
7.09814633450196));
#12416=CARTESIAN_POINT('Ctrl Pts',(0.402960792325747,-2.90585094023315,
7.16634457332539));
#12417=CARTESIAN_POINT('Ctrl Pts',(0.835793473763965,-2.95184458747716,
7.59911373795158));
#12418=CARTESIAN_POINT('Ctrl Pts',(0.893222610079682,-2.99022150713542,
8.1059459436348));
#12419=CARTESIAN_POINT('Ctrl Pts',(0.742230061053853,-3.02094600804868,
8.46767578677156));
#12420=CARTESIAN_POINT('Ctrl Pts',(0.525050043132394,-3.04656270442428,
8.7112819718791));
#12421=CARTESIAN_POINT('Ctrl Pts',(0.197561468846462,-3.07475163348297,
8.86898675520401));
#12422=CARTESIAN_POINT('Ctrl Pts',(-0.198942516484079,-3.10552114011045,
8.86910705024245));
#12423=CARTESIAN_POINT('Ctrl Pts',(-0.556404604870121,-3.13629694361956,
8.69691854995843));
#12424=CARTESIAN_POINT('Ctrl Pts',(-0.803908575128165,-3.16708632463838,
8.38679365490788));
#12425=CARTESIAN_POINT('Ctrl Pts',(-0.892230210331149,-3.19787639573897,
7.99981674999116));
#12426=CARTESIAN_POINT('Ctrl Pts',(-0.811254302996053,-3.22610486728836,
7.64504873212211));
#12427=CARTESIAN_POINT('Ctrl Pts',(-0.621751910267926,-3.25176808988285,
7.37851925540117));
#12428=CARTESIAN_POINT('Ctrl Pts',(-0.301953097190216,-3.28256284856841,
7.15059667963661));
#12429=CARTESIAN_POINT('Ctrl Pts',(0.206209630770826,-3.32104498703397,
7.092565584774));
#12430=CARTESIAN_POINT('Ctrl Pts',(0.726383216812123,-3.36720427357741,
7.41989946778657));
#12431=CARTESIAN_POINT('Ctrl Pts',(0.861157216643285,-3.39796397231344,
7.80525499237318));
#12432=CARTESIAN_POINT('Ctrl Pts',(0.861183614424057,-3.41333048413908,
7.99893401904505));
#12433=CARTESIAN_POINT('Ctrl Pts',(0.799999353205571,-2.14018795858917,
8.00474549279328));
#12434=CARTESIAN_POINT('Ctrl Pts',(0.799974799734663,-2.15448086801293,
8.18489286877592));
#12435=CARTESIAN_POINT('Ctrl Pts',(0.674665007466417,-2.18310389914977,
8.54360793631645));
#12436=CARTESIAN_POINT('Ctrl Pts',(0.189057319427946,-2.22621797906703,
8.84931316013818));
#12437=CARTESIAN_POINT('Ctrl Pts',(-0.382526459311769,-2.26949883233014,
8.78512361823764));
#12438=CARTESIAN_POINT('Ctrl Pts',(-0.807840639236961,-2.31455899583364,
8.36128354752488));
#12439=CARTESIAN_POINT('Ctrl Pts',(-0.841884630553248,-2.34849059789531,
7.90616153590567));
#12440=CARTESIAN_POINT('Ctrl Pts',(-0.706633312481697,-2.3776482221266,
7.56417102566761));
#12441=CARTESIAN_POINT('Ctrl Pts',(-0.524797421299121,-2.40036397277687,
7.33517763260607));
#12442=CARTESIAN_POINT('Ctrl Pts',(-0.184623097405697,-2.42964203470304,
7.17129916558269));
#12443=CARTESIAN_POINT('Ctrl Pts',(0.193484153574259,-2.4589910981866,7.17122122775637));
#12444=CARTESIAN_POINT('Ctrl Pts',(0.53519122257586,-2.48841027946974,7.33563982396839));
#12445=CARTESIAN_POINT('Ctrl Pts',(0.772150285550503,-2.51789845810207,
7.63264106317873));
#12446=CARTESIAN_POINT('Ctrl Pts',(0.857109363647141,-2.54745448449862,
8.00408762003218));
#12447=CARTESIAN_POINT('Ctrl Pts',(0.772052203859602,-2.5770771143395,8.37600483173473));
#12448=CARTESIAN_POINT('Ctrl Pts',(0.507269008134946,-2.61006365580992,
8.70902087610833));
#12449=CARTESIAN_POINT('Ctrl Pts',(0.184121132841334,-2.63651910824196,
8.83624322508014));
#12450=CARTESIAN_POINT('Ctrl Pts',(-0.066489483803979,-2.65639505342702,
8.83575881359142));
#12451=CARTESIAN_POINT('Ctrl Pts',(-0.272993262404685,-2.67296969383809,
8.80486180272118));
#12452=CARTESIAN_POINT('Ctrl Pts',(-0.542963798600168,-2.69620569938568,
8.6749478571166));
#12453=CARTESIAN_POINT('Ctrl Pts',(-0.783400610994973,-2.72613969346878,
8.3735180635455));
#12454=CARTESIAN_POINT('Ctrl Pts',(-0.884539863210645,-2.76112964475965,
7.93383176138089));
#12455=CARTESIAN_POINT('Ctrl Pts',(-0.709496036003296,-2.80121083689286,
7.43066574821048));
#12456=CARTESIAN_POINT('Ctrl Pts',(-0.200096069822599,-2.84642092016874,
7.11042023888795));
#12457=CARTESIAN_POINT('Ctrl Pts',(0.398680163779428,-2.89174303462223,
7.17762409038781));
#12458=CARTESIAN_POINT('Ctrl Pts',(0.826194257186495,-2.93717015873569,
7.60494403903258));
#12459=CARTESIAN_POINT('Ctrl Pts',(0.883028763967666,-2.97510749619044,
8.10591734828594));
#12460=CARTESIAN_POINT('Ctrl Pts',(0.733685094600885,-3.00550240345549,
8.46374186218363));
#12461=CARTESIAN_POINT('Ctrl Pts',(0.518762431301621,-3.03085542203816,
8.70482943573385));
#12462=CARTESIAN_POINT('Ctrl Pts',(0.194479876070813,-3.05877306117867,
8.86101946641206));
#12463=CARTESIAN_POINT('Ctrl Pts',(-0.198398854087579,-3.08926279897463,
8.86116295997746));
#12464=CARTESIAN_POINT('Ctrl Pts',(-0.552866770740287,-3.11978430147565,
8.69045288806385));
#12465=CARTESIAN_POINT('Ctrl Pts',(-0.798459570530803,-3.15033499607393,
8.38276097552609));
#12466=CARTESIAN_POINT('Ctrl Pts',(-0.886189886223361,-3.18091257250085,
7.9985222617957));
#12467=CARTESIAN_POINT('Ctrl Pts',(-0.805754444707439,-3.20896404488721,
7.64600910454789));
#12468=CARTESIAN_POINT('Ctrl Pts',(-0.617356025266483,-3.23448146889928,
7.38101130632405));
#12469=CARTESIAN_POINT('Ctrl Pts',(-0.299249903140631,-3.2651162608211,
7.15427322620025));
#12470=CARTESIAN_POINT('Ctrl Pts',(0.20669102063405,-3.30343842772452,7.09641469177514));
#12471=CARTESIAN_POINT('Ctrl Pts',(0.72520383869486,-3.34944736574065,7.4225450742071));
#12472=CARTESIAN_POINT('Ctrl Pts',(0.859802571238952,-3.38014846116659,
7.80703861326121));
#12473=CARTESIAN_POINT('Ctrl Pts',(0.859828918911975,-3.39548580458109,
8.00035000220606));
#12474=CARTESIAN_POINT('Ctrl Pts',(0.753146974179187,-2.1619943924303,8.27380160983776));
#12475=CARTESIAN_POINT('Ctrl Pts',(0.723482246295192,-2.16903452865882,
8.35718646810225));
#12476=CARTESIAN_POINT('Ctrl Pts',(0.680269466184233,-2.17608055625528,
8.43571695267455));
#12477=CARTESIAN_POINT('Ctrl Pts',(0.6250578408604,-2.18313382135177,8.50488004006827));
#12478=CARTESIAN_POINT('Ctrl Pts',(0.51279577812026,-2.19747525912219,8.64550967759036));
#12479=CARTESIAN_POINT('Ctrl Pts',(0.350926548774103,-2.21184661909461,
8.74741141886427));
#12480=CARTESIAN_POINT('Ctrl Pts',(0.174727970977739,-2.22624577462467,
8.7876640325178));
#12481=CARTESIAN_POINT('Ctrl Pts',(-0.00147060681862579,-2.24064493015473,
8.82791664617134));
#12482=CARTESIAN_POINT('Ctrl Pts',(-0.191998533065198,-2.25507188124244,
8.80652013220449));
#12483=CARTESIAN_POINT('Ctrl Pts',(-0.355616560819318,-2.26952716877793,
8.72770472099937));
#12484=CARTESIAN_POINT('Ctrl Pts',(-0.519234588573438,-2.28398245631341,
8.64888930979425));
#12485=CARTESIAN_POINT('Ctrl Pts',(-0.655942717835107,-2.29846608029668,
8.51265500135086));
#12486=CARTESIAN_POINT('Ctrl Pts',(-0.734805551021998,-2.31297741063122,
8.34855954342037));
#12487=CARTESIAN_POINT('Ctrl Pts',(-0.822430921229655,-2.32910111100293,
8.16623125683093));
#12488=CARTESIAN_POINT('Ctrl Pts',(-0.838642345665982,-2.34525901674658,
7.94950648939321));
#12489=CARTESIAN_POINT('Ctrl Pts',(-0.778727898779652,-2.36145090114427,
7.75505675489523));
#12490=CARTESIAN_POINT('Ctrl Pts',(-0.766745009402386,-2.36468927802381,
7.71616680799563));
#12491=CARTESIAN_POINT('Ctrl Pts',(-0.751717085172214,-2.3679290140495,
7.67816786241363));
#12492=CARTESIAN_POINT('Ctrl Pts',(-0.733952003028779,-2.37117009287772,
7.64149031776064));
#12493=CARTESIAN_POINT('Ctrl Pts',(-0.680656756598472,-2.38089332936235,
7.53145768380167));
#12494=CARTESIAN_POINT('Ctrl Pts',(-0.602727088948797,-2.39062865106961,
7.43331765820387));
#12495=CARTESIAN_POINT('Ctrl Pts',(-0.507066534475055,-2.40037598891093,
7.35693456756774));
#12496=CARTESIAN_POINT('Ctrl Pts',(-0.411405980001313,-2.41012332675226,
7.28055147693161));
#12497=CARTESIAN_POINT('Ctrl Pts',(-0.298014538703504,-2.41988268072765,
7.22592532125715));
#12498=CARTESIAN_POINT('Ctrl Pts',(-0.178300942891275,-2.42965386829594,
7.1985992537822));
#12499=CARTESIAN_POINT('Ctrl Pts',(-0.0585873470790449,-2.43942505586423,
7.17127318630725));
#12500=CARTESIAN_POINT('Ctrl Pts',(0.0674484032476069,-2.44920807702541,
7.17124720703181));
#12501=CARTESIAN_POINT('Ctrl Pts',(0.187417456577866,-2.45900278448653,
7.19863731676276));
#12502=CARTESIAN_POINT('Ctrl Pts',(0.307386509908125,-2.46879749194765,
7.22602742649371));
#12503=CARTESIAN_POINT('Ctrl Pts',(0.421288866241992,-2.4786038857087,7.28083362523105));
#12504=CARTESIAN_POINT('Ctrl Pts',(0.517733221571367,-2.48842177902794,
7.35773693113477));
#12505=CARTESIAN_POINT('Ctrl Pts',(0.61417757690074,-2.49823967234718,7.4346402370385));
#12506=CARTESIAN_POINT('Ctrl Pts',(0.693163931225622,-2.50806906522463,
7.53364065010862));
#12507=CARTESIAN_POINT('Ctrl Pts',(0.746816954737502,-2.51790976606277,
7.64504861611925));
#12508=CARTESIAN_POINT('Ctrl Pts',(0.800469978249382,-2.52775046690092,
7.75645658212988));
#12509=CARTESIAN_POINT('Ctrl Pts',(0.828789670948262,-2.53760247569977,
7.88027210108103));
#12510=CARTESIAN_POINT('Ctrl Pts',(0.828773323999778,-2.54746558507267,
8.00416606250703));
#12511=CARTESIAN_POINT('Ctrl Pts',(0.828756977051295,-2.55732869444558,
8.12806002393303));
#12512=CARTESIAN_POINT('Ctrl Pts',(0.800404590455449,-2.56720290439254,
8.25203242783388));
#12513=CARTESIAN_POINT('Ctrl Pts',(0.746510917798827,-2.57708799058658,
8.36397103644034));
#12514=CARTESIAN_POINT('Ctrl Pts',(0.692617245142206,-2.58697307678063,
8.47590964504681));
#12515=CARTESIAN_POINT('Ctrl Pts',(0.613182286424809,-2.59686903922175,
8.57581445835889));
#12516=CARTESIAN_POINT('Ctrl Pts',(0.515856401485537,-2.60677564404326,
8.65334937205055));
#12517=CARTESIAN_POINT('Ctrl Pts',(0.386088554899842,-2.61998445047194,
8.75672925697275));
#12518=CARTESIAN_POINT('Ctrl Pts',(0.224514617253036,-2.63321217668796,
8.82034043145866));
#12519=CARTESIAN_POINT('Ctrl Pts',(0.0585408341795072,-2.64645822602986,
8.83280431356186));
#12520=CARTESIAN_POINT('Ctrl Pts',(0.0170473884111253,-2.64976973836533,
8.83592028408766));
#12521=CARTESIAN_POINT('Ctrl Pts',(-0.0247210476964266,-2.65308239589618,
8.83583954883954));
#12522=CARTESIAN_POINT('Ctrl Pts',(-0.0662556436102732,-2.6563961887027,
8.83270948012845));
#12523=CARTESIAN_POINT('Ctrl Pts',(-0.10779023952412,-2.65970998150923,
8.82957941141737));
#12524=CARTESIAN_POINT('Ctrl Pts',(-0.149090995244261,-2.66302490959145,
8.82340000924332));
#12525=CARTESIAN_POINT('Ctrl Pts',(-0.189708366898492,-2.66634096299409,
8.81412567384119));
#12526=CARTESIAN_POINT('Ctrl Pts',(-0.311560481861183,-2.67628912320203,
8.78630266763481));
#12527=CARTESIAN_POINT('Ctrl Pts',(-0.427262140230675,-2.68624741129386,
8.73062526237571));
#12528=CARTESIAN_POINT('Ctrl Pts',(-0.525185771481222,-2.69621555435362,
8.65254826081764));
#12529=CARTESIAN_POINT('Ctrl Pts',(-0.623109402731769,-2.70618369741338,
8.57447125925957));
#12530=CARTESIAN_POINT('Ctrl Pts',(-0.703255006863371,-2.71616169544108,
8.47399466140254));
#12531=CARTESIAN_POINT('Ctrl Pts',(-0.757776273531411,-2.72614925892505,
8.36094403359336));
#12532=CARTESIAN_POINT('Ctrl Pts',(-0.81229754019945,-2.73613682240903,
8.24789340578418));
#12533=CARTESIAN_POINT('Ctrl Pts',(-0.841194469403928,-2.74613395134928,
8.12226874802287));
#12534=CARTESIAN_POINT('Ctrl Pts',(-0.84102824420588,-2.75614034792675,
7.99657735204903));
#12535=CARTESIAN_POINT('Ctrl Pts',(-0.840778906408808,-2.77114994279295,
7.80804025808828));
#12536=CARTESIAN_POINT('Ctrl Pts',(-0.775137471206052,-2.7861803898429,
7.61935300314938));
#12537=CARTESIAN_POINT('Ctrl Pts',(-0.657416759241225,-2.8012306272472,
7.47163512412617));
#12538=CARTESIAN_POINT('Ctrl Pts',(-0.539696047276397,-2.81628086465149,
7.32391724510297));
#12539=CARTESIAN_POINT('Ctrl Pts',(-0.369896058549498,-2.83135089241011,
7.21716874199546));
#12540=CARTESIAN_POINT('Ctrl Pts',(-0.185200025252378,-2.84643959203168,
7.17499513235835));
#12541=CARTESIAN_POINT('Ctrl Pts',(-0.000503991955257244,-2.86152829165324,
7.13282152272124));
#12542=CARTESIAN_POINT('Ctrl Pts',(0.199088085912085,-2.87663566313774,
7.15522280655453));
#12543=CARTESIAN_POINT('Ctrl Pts',(0.370136473746934,-2.89176053623223,
7.23764343991196));
#12544=CARTESIAN_POINT('Ctrl Pts',(0.541184861581783,-2.90688540932672,
7.3200640732694));
#12545=CARTESIAN_POINT('Ctrl Pts',(0.683689559384138,-2.92202778403121,
7.46250405615099));
#12546=CARTESIAN_POINT('Ctrl Pts',(0.766308809641551,-2.9371864388744,7.63391870944245));
#12547=CARTESIAN_POINT('Ctrl Pts',(0.848928059898963,-2.95234509371759,
7.80533336273392));
#12548=CARTESIAN_POINT('Ctrl Pts',(0.871661862611432,-2.96752002869949,
8.00572268643527));
#12549=CARTESIAN_POINT('Ctrl Pts',(0.829458573726661,-2.98270997611514,
8.19179396563495));
#12550=CARTESIAN_POINT('Ctrl Pts',(0.808356929284276,-2.99030494982297,
8.28482960523479));
#12551=CARTESIAN_POINT('Ctrl Pts',(0.77102101194258,-2.99790367663923,8.37428573370921));
#12552=CARTESIAN_POINT('Ctrl Pts',(0.720114653776843,-3.00550599283476,
8.45517693397895));
#12553=CARTESIAN_POINT('Ctrl Pts',(0.669208295611106,-3.01310830903029,
8.5360681342487));
#12554=CARTESIAN_POINT('Ctrl Pts',(0.604731496621327,-3.02071421460509,
8.60839440631376));
#12555=CARTESIAN_POINT('Ctrl Pts',(0.529984455678112,-3.02832354704088,
8.66797968224839));
#12556=CARTESIAN_POINT('Ctrl Pts',(0.430321734420493,-3.03846932362193,
8.7474267168279));
#12557=CARTESIAN_POINT('Ctrl Pts',(0.312400805245652,-3.0486211924003,8.80422309161998));
#12558=CARTESIAN_POINT('Ctrl Pts',(0.187960552298501,-3.05877874975548,
8.83264519461025));
#12559=CARTESIAN_POINT('Ctrl Pts',(0.0635202993513489,-3.06893630711065,
8.86106729760052));
#12560=CARTESIAN_POINT('Ctrl Pts',(-0.0674392773681153,-3.07909955304264,
8.86111512878899));
#12561=CARTESIAN_POINT('Ctrl Pts',(-0.191997051836632,-3.08926809309214,
8.83268736573095));
#12562=CARTESIAN_POINT('Ctrl Pts',(-0.316554826305149,-3.09943663314163,
8.80425960267292));
#12563=CARTESIAN_POINT('Ctrl Pts',(-0.434710798522717,-3.10961046730864,
8.74735624536838));
#12564=CARTESIAN_POINT('Ctrl Pts',(-0.534720917929921,-3.11978916682519,
8.66762258129316));
#12565=CARTESIAN_POINT('Ctrl Pts',(-0.634731037337125,-3.12996786634175,
8.58788891721793));
#12566=CARTESIAN_POINT('Ctrl Pts',(-0.716595303933964,-3.14015143120784,
8.48532494637201));
#12567=CARTESIAN_POINT('Ctrl Pts',(-0.772149156514476,-3.1503394763787,
8.37000317532732));
#12568=CARTESIAN_POINT('Ctrl Pts',(-0.827703009094989,-3.16052752154957,
8.25468140428263));
#12569=CARTESIAN_POINT('Ctrl Pts',(-0.856946447659175,-3.17072004702521,
8.12660183303916));
#12570=CARTESIAN_POINT('Ctrl Pts',(-0.8569435412111,-3.18091657746964,7.99846874609965));
#12571=CARTESIAN_POINT('Ctrl Pts',(-0.856940634763026,-3.19111310791407,
7.87033565916013));
#12572=CARTESIAN_POINT('Ctrl Pts',(-0.82769138330269,-3.20131364332729,
7.74214905652457));
#12573=CARTESIAN_POINT('Ctrl Pts',(-0.772093493947471,-3.21151785542143,
7.62664101580102));
#12574=CARTESIAN_POINT('Ctrl Pts',(-0.730395076931056,-3.21917101449204,
7.54000998525836));
#12575=CARTESIAN_POINT('Ctrl Pts',(-0.67387555109877,-3.22682624169566,
7.4605106457912));
#12576=CARTESIAN_POINT('Ctrl Pts',(-0.605852522916895,-3.2344832042877,
7.39241871604215));
#12577=CARTESIAN_POINT('Ctrl Pts',(-0.53782949473502,-3.24214016687973,
7.3243267862931));
#12578=CARTESIAN_POINT('Ctrl Pts',(-0.458302964203557,-3.24979886486019,
7.26764226626215));
#12579=CARTESIAN_POINT('Ctrl Pts',(-0.37155588226427,-3.25745947464072,
7.22599535061318));
#12580=CARTESIAN_POINT('Ctrl Pts',(-0.198061718385695,-3.27278069420178,
7.14270151931523));
#12581=CARTESIAN_POINT('Ctrl Pts',(0.00431465112417784,-3.28810956096315,
7.11955810554519));
#12582=CARTESIAN_POINT('Ctrl Pts',(0.191921638889249,-3.30344215067986,
7.16234146239883));
#12583=CARTESIAN_POINT('Ctrl Pts',(0.37952862665432,-3.31877474039656,7.20512481925246));
#12584=CARTESIAN_POINT('Ctrl Pts',(0.55236623267459,-3.33411105306861,7.31383494672978));
#12585=CARTESIAN_POINT('Ctrl Pts',(0.672434718820748,-3.34945448326111,
7.46431339523197));
#12586=CARTESIAN_POINT('Ctrl Pts',(0.780125650037461,-3.36321619824999,
7.59927940311118));
#12587=CARTESIAN_POINT('Ctrl Pts',(0.845366351460771,-3.37698363894322,
7.76784602494453));
#12588=CARTESIAN_POINT('Ctrl Pts',(0.857691923859112,-3.39074214267724,
7.9406445962268));
#12589=CARTESIAN_POINT('',(0.,0.,0.));
#12590=CARTESIAN_POINT('Origin',(0.115470053837925,-0.5,-0.2));
#12591=CARTESIAN_POINT('',(0.23094010767585,-0.5,0.));
#12592=CARTESIAN_POINT('',(0.115470053837925,-0.5,-0.2));
#12593=CARTESIAN_POINT('',(0.23094010767585,-0.5,0.));
#12594=CARTESIAN_POINT('',(0.115470053837925,-0.8,-0.2));
#12595=CARTESIAN_POINT('',(0.115470053837925,-0.5,-0.2));
#12596=CARTESIAN_POINT('',(0.23094010767585,-0.8,0.));
#12597=CARTESIAN_POINT('',(0.23094010767585,-0.8,0.));
#12598=CARTESIAN_POINT('',(0.23094010767585,-0.5,0.));
#12599=CARTESIAN_POINT('Origin',(-0.115470053837925,-0.5,-0.2));
#12600=CARTESIAN_POINT('',(-0.115470053837925,-0.5,-0.2));
#12601=CARTESIAN_POINT('',(0.115470053837925,-0.5,-0.2));
#12602=CARTESIAN_POINT('',(-0.115470053837925,-0.8,-0.2));
#12603=CARTESIAN_POINT('',(-0.115470053837925,-0.5,-0.2));
#12604=CARTESIAN_POINT('',(0.115470053837925,-0.8,-0.2));
#12605=CARTESIAN_POINT('Origin',(-0.23094010767585,-0.5,-2.77555756156289E-17));
#12606=CARTESIAN_POINT('',(-0.23094010767585,-0.5,-2.82820063659975E-17));
#12607=CARTESIAN_POINT('',(-0.115470053837925,-0.5,-0.2));
#12608=CARTESIAN_POINT('',(-0.23094010767585,-0.8,-2.77555756156289E-17));
#12609=CARTESIAN_POINT('',(-0.23094010767585,-0.5,-2.82820063659975E-17));
#12610=CARTESIAN_POINT('',(-0.115470053837925,-0.8,-0.2));
#12611=CARTESIAN_POINT('Origin',(-0.115470053837925,-0.5,0.2));
#12612=CARTESIAN_POINT('',(-0.115470053837925,-0.5,0.2));
#12613=CARTESIAN_POINT('',(-0.23094010767585,-0.5,-2.82820063659975E-17));
#12614=CARTESIAN_POINT('',(-0.115470053837925,-0.8,0.2));
#12615=CARTESIAN_POINT('',(-0.115470053837925,-0.5,0.2));
#12616=CARTESIAN_POINT('',(-0.23094010767585,-0.8,-2.82820063659975E-17));
#12617=CARTESIAN_POINT('Origin',(0.115470053837925,-0.5,0.2));
#12618=CARTESIAN_POINT('',(0.115470053837925,-0.5,0.2));
#12619=CARTESIAN_POINT('',(-0.115470053837925,-0.5,0.2));
#12620=CARTESIAN_POINT('',(0.115470053837925,-0.8,0.2));
#12621=CARTESIAN_POINT('',(0.115470053837925,-0.5,0.2));
#12622=CARTESIAN_POINT('',(-0.115470053837925,-0.8,0.2));
#12623=CARTESIAN_POINT('Origin',(0.23094010767585,-0.5,0.));
#12624=CARTESIAN_POINT('',(0.115470053837925,-0.5,0.2));
#12625=CARTESIAN_POINT('',(0.115470053837925,-0.8,0.2));
#12626=CARTESIAN_POINT('Origin',(0.,-0.5,0.));
#12627=CARTESIAN_POINT('Origin',(0.,-0.8,0.));
#12628=CARTESIAN_POINT('Origin',(0.,-1.4,0.));
#12629=CARTESIAN_POINT('',(-0.24505,-1.4,3.00099698131059E-17));
#12630=CARTESIAN_POINT('Origin',(0.,-1.4,0.));
#12631=CARTESIAN_POINT('Origin',(0.375,0.5,0.));
#12632=CARTESIAN_POINT('',(-0.375,0.5,-4.59242549680257E-17));
#12633=CARTESIAN_POINT('Origin',(0.,0.5,0.));
#12634=CARTESIAN_POINT('Origin',(0.,0.475,0.));
#12635=CARTESIAN_POINT('',(-0.425,0.45,-5.20474889637625E-17));
#12636=CARTESIAN_POINT('Origin',(0.,0.45,0.));
#12637=CARTESIAN_POINT('',(-0.4,0.475,-4.89858719658941E-17));
#12638=CARTESIAN_POINT('Origin',(0.,0.24,0.));
#12639=CARTESIAN_POINT('',(-0.425,0.0299999999999998,-5.20474889637625E-17));
#12640=CARTESIAN_POINT('Origin',(0.,0.0299999999999998,0.));
#12641=CARTESIAN_POINT('',(-0.425,0.24,-5.20474889637625E-17));
#12642=CARTESIAN_POINT('Origin',(0.,0.0150000000000001,0.));
#12643=CARTESIAN_POINT('',(-0.395,4.85722573273506E-17,-4.83735485663204E-17));
#12644=CARTESIAN_POINT('Origin',(0.,0.,0.));
#12645=CARTESIAN_POINT('',(-0.41,0.0150000000000001,-5.02105187650415E-17));
#12646=CARTESIAN_POINT('Origin',(0.27,0.,0.));
#12647=CARTESIAN_POINT('',(-0.27,0.,-3.30654635769785E-17));
#12648=CARTESIAN_POINT('Origin',(0.,0.,0.));
#12649=CARTESIAN_POINT('Origin',(0.,-0.02,0.));
#12650=CARTESIAN_POINT('',(-0.24505,-0.0498999999999999,3.00099698131059E-17));
#12651=CARTESIAN_POINT('Origin',(0.,-0.0498999999999999,0.));
#12652=CARTESIAN_POINT('',(-0.26,-0.02,-3.18408167778312E-17));
#12653=CARTESIAN_POINT('Origin',(0.,-0.995,0.));
#12654=CARTESIAN_POINT('',(-0.24505,-0.995,-3.00099698131059E-17));
#12655=CARTESIAN_POINT('',(0.,0.,0.));
#12656=CARTESIAN_POINT('',(0.,0.,0.));
#12657=CARTESIAN_POINT('Origin',(18.7625631329235,-1.15,6.76256313292354));
#12658=CARTESIAN_POINT('',(18.5975631329235,-1.05,6.76256313292354));
#12659=CARTESIAN_POINT('Origin',(18.7625631329235,-1.05,6.76256313292354));
#12660=CARTESIAN_POINT('',(18.5975631329235,1.05,6.76256313292354));
#12661=CARTESIAN_POINT('',(18.5975631329235,-1.15,6.76256313292354));
#12662=CARTESIAN_POINT('Origin',(18.7625631329235,1.05,6.76256313292354));
#12663=CARTESIAN_POINT('Origin',(18.7625631329235,-1.15,9.23743686707646));
#12664=CARTESIAN_POINT('',(18.5975631329235,-1.05,9.23743686707646));
#12665=CARTESIAN_POINT('Origin',(18.7625631329235,-1.05,9.23743686707646));
#12666=CARTESIAN_POINT('',(18.5975631329235,1.05,9.23743686707646));
#12667=CARTESIAN_POINT('',(18.5975631329235,-1.15,9.23743686707646));
#12668=CARTESIAN_POINT('Origin',(18.7625631329235,1.05,9.23743686707646));
#12669=CARTESIAN_POINT('Origin',(21.2374368670765,-1.15,9.23743686707646));
#12670=CARTESIAN_POINT('',(21.0724368670765,-1.05,9.23743686707646));
#12671=CARTESIAN_POINT('Origin',(21.2374368670765,-1.05,9.23743686707646));
#12672=CARTESIAN_POINT('',(21.0724368670765,1.05,9.23743686707646));
#12673=CARTESIAN_POINT('',(21.0724368670765,-1.15,9.23743686707646));
#12674=CARTESIAN_POINT('Origin',(21.2374368670765,1.05,9.23743686707646));
#12675=CARTESIAN_POINT('Origin',(21.2374368670765,-1.15,6.76256313292354));
#12676=CARTESIAN_POINT('',(21.0724368670765,-1.05,6.76256313292354));
#12677=CARTESIAN_POINT('Origin',(21.2374368670765,-1.05,6.76256313292354));
#12678=CARTESIAN_POINT('',(21.0724368670765,1.05,6.76256313292354));
#12679=CARTESIAN_POINT('',(21.0724368670765,-1.15,6.76256313292354));
#12680=CARTESIAN_POINT('Origin',(21.2374368670765,1.05,6.76256313292354));
#12681=CARTESIAN_POINT('Origin',(-1.23743686707646,-1.15,6.76256313292354));
#12682=CARTESIAN_POINT('',(-1.40243686707646,-1.05,6.76256313292354));
#12683=CARTESIAN_POINT('Origin',(-1.23743686707646,-1.05,6.76256313292354));
#12684=CARTESIAN_POINT('',(-1.40243686707646,1.05,6.76256313292354));
#12685=CARTESIAN_POINT('',(-1.40243686707646,-1.15,6.76256313292354));
#12686=CARTESIAN_POINT('Origin',(-1.23743686707646,1.05,6.76256313292354));
#12687=CARTESIAN_POINT('Origin',(-1.23743686707646,-1.15,9.23743686707646));
#12688=CARTESIAN_POINT('',(-1.40243686707646,-1.05,9.23743686707646));
#12689=CARTESIAN_POINT('Origin',(-1.23743686707646,-1.05,9.23743686707646));
#12690=CARTESIAN_POINT('',(-1.40243686707646,1.05,9.23743686707646));
#12691=CARTESIAN_POINT('',(-1.40243686707646,-1.15,9.23743686707646));
#12692=CARTESIAN_POINT('Origin',(-1.23743686707646,1.05,9.23743686707646));
#12693=CARTESIAN_POINT('Origin',(1.23743686707646,-1.15,9.23743686707646));
#12694=CARTESIAN_POINT('',(1.07243686707646,-1.05,9.23743686707646));
#12695=CARTESIAN_POINT('Origin',(1.23743686707646,-1.05,9.23743686707646));
#12696=CARTESIAN_POINT('',(1.07243686707646,1.05,9.23743686707646));
#12697=CARTESIAN_POINT('',(1.07243686707646,-1.15,9.23743686707646));
#12698=CARTESIAN_POINT('Origin',(1.23743686707646,1.05,9.23743686707646));
#12699=CARTESIAN_POINT('Origin',(1.23743686707646,-1.15,6.76256313292354));
#12700=CARTESIAN_POINT('',(1.07243686707646,-1.05,6.76256313292354));
#12701=CARTESIAN_POINT('Origin',(1.23743686707646,-1.05,6.76256313292354));
#12702=CARTESIAN_POINT('',(1.07243686707646,1.05,6.76256313292354));
#12703=CARTESIAN_POINT('',(1.07243686707646,-1.15,6.76256313292354));
#12704=CARTESIAN_POINT('Origin',(1.23743686707646,1.05,6.76256313292354));
#12705=CARTESIAN_POINT('Origin',(0.,-1.15,8.));
#12706=CARTESIAN_POINT('',(-1.5,-1.05,8.));
#12707=CARTESIAN_POINT('Origin',(0.,-1.05,8.));
#12708=CARTESIAN_POINT('',(-1.5,1.05,8.));
#12709=CARTESIAN_POINT('',(-1.5,-1.15,8.));
#12710=CARTESIAN_POINT('Origin',(0.,1.05,8.));
#12711=CARTESIAN_POINT('Origin',(20.,-1.15,8.));
#12712=CARTESIAN_POINT('',(18.5,-1.05,8.));
#12713=CARTESIAN_POINT('Origin',(20.,-1.05,8.));
#12714=CARTESIAN_POINT('',(18.5,1.05,8.));
#12715=CARTESIAN_POINT('',(18.5,-1.15,8.));
#12716=CARTESIAN_POINT('Origin',(20.,1.05,8.));
#12717=CARTESIAN_POINT('Origin',(20.,-1.05,8.));
#12718=CARTESIAN_POINT('',(17.9506098468081,1.05,7.2));
#12719=CARTESIAN_POINT('',(17.9506098468081,-1.05,7.2));
#12720=CARTESIAN_POINT('',(17.9506098468081,-1.05,7.2));
#12721=CARTESIAN_POINT('',(17.9506098468081,1.05,8.8));
#12722=CARTESIAN_POINT('Origin',(20.,1.05,8.));
#12723=CARTESIAN_POINT('',(17.9506098468081,-1.05,8.8));
#12724=CARTESIAN_POINT('',(17.9506098468081,-1.05,8.8));
#12725=CARTESIAN_POINT('Origin',(20.,-1.05,8.));
#12726=CARTESIAN_POINT('Origin',(20.,-1.05,7.2));
#12727=CARTESIAN_POINT('',(2.04939015319192,-1.05,7.2));
#12728=CARTESIAN_POINT('',(0.,-1.05,7.2));
#12729=CARTESIAN_POINT('',(2.04939015319192,1.05,7.2));
#12730=CARTESIAN_POINT('',(2.04939015319192,-1.05,7.2));
#12731=CARTESIAN_POINT('',(0.,1.05,7.2));
#12732=CARTESIAN_POINT('Origin',(0.,-1.05,8.));
#12733=CARTESIAN_POINT('',(2.04939015319192,-1.05,8.8));
#12734=CARTESIAN_POINT('',(20.,-1.05,8.8));
#12735=CARTESIAN_POINT('Origin',(0.,-1.05,8.));
#12736=CARTESIAN_POINT('Origin',(0.,-1.05,8.8));
#12737=CARTESIAN_POINT('',(2.04939015319192,1.05,8.8));
#12738=CARTESIAN_POINT('',(20.,1.05,8.8));
#12739=CARTESIAN_POINT('',(2.04939015319192,-1.05,8.8));
#12740=CARTESIAN_POINT('Origin',(0.,-1.05,8.));
#12741=CARTESIAN_POINT('Origin',(0.,1.05,8.));
#12742=CARTESIAN_POINT('Origin',(0.,1.05,8.));
#12743=CARTESIAN_POINT('',(0.,0.,0.));
#12744=CARTESIAN_POINT('Origin',(0.,-0.15,8.));
#12745=CARTESIAN_POINT('',(-1.02,0.15,8.));
#12746=CARTESIAN_POINT('Origin',(0.,0.15,8.));
#12747=CARTESIAN_POINT('',(-1.02,-0.15,8.));
#12748=CARTESIAN_POINT('',(-1.02,-0.15,8.));
#12749=CARTESIAN_POINT('Origin',(0.,-0.15,8.));
#12750=CARTESIAN_POINT('Origin',(0.,-0.15,8.));
#12751=CARTESIAN_POINT('',(-1.49,0.15,8.));
#12752=CARTESIAN_POINT('Origin',(0.,0.15,8.));
#12753=CARTESIAN_POINT('',(-1.49,-0.15,8.));
#12754=CARTESIAN_POINT('',(-1.49,-0.15,8.));
#12755=CARTESIAN_POINT('Origin',(0.,-0.15,8.));
#12756=CARTESIAN_POINT('Origin',(0.,0.15,8.));
#12757=CARTESIAN_POINT('Origin',(0.,-0.15,8.));
#12758=CARTESIAN_POINT('',(0.,0.,0.));
#12759=CARTESIAN_POINT('Origin',(-1.23743686707646,-1.5,6.76256313292354));
#12760=CARTESIAN_POINT('',(-1.46243686707646,-1.4,6.76256313292354));
#12761=CARTESIAN_POINT('Origin',(-1.23743686707646,-1.4,6.76256313292354));
#12762=CARTESIAN_POINT('',(-1.46243686707646,-1.05,6.76256313292354));
#12763=CARTESIAN_POINT('',(-1.46243686707646,-1.5,6.76256313292354));
#12764=CARTESIAN_POINT('Origin',(-1.23743686707646,-1.05,6.76256313292354));
#12765=CARTESIAN_POINT('Origin',(-1.23743686707646,-1.5,9.23743686707646));
#12766=CARTESIAN_POINT('',(-1.46243686707646,-1.4,9.23743686707646));
#12767=CARTESIAN_POINT('Origin',(-1.23743686707646,-1.4,9.23743686707646));
#12768=CARTESIAN_POINT('',(-1.46243686707646,-1.05,9.23743686707646));
#12769=CARTESIAN_POINT('',(-1.46243686707646,-1.5,9.23743686707646));
#12770=CARTESIAN_POINT('Origin',(-1.23743686707646,-1.05,9.23743686707646));
#12771=CARTESIAN_POINT('Origin',(1.23743686707646,-1.5,9.23743686707646));
#12772=CARTESIAN_POINT('',(1.01243686707646,-1.4,9.23743686707646));
#12773=CARTESIAN_POINT('Origin',(1.23743686707646,-1.4,9.23743686707646));
#12774=CARTESIAN_POINT('',(1.01243686707646,-1.05,9.23743686707646));
#12775=CARTESIAN_POINT('',(1.01243686707646,-1.5,9.23743686707646));
#12776=CARTESIAN_POINT('Origin',(1.23743686707646,-1.05,9.23743686707646));
#12777=CARTESIAN_POINT('Origin',(1.23743686707646,-1.5,6.76256313292354));
#12778=CARTESIAN_POINT('',(1.01243686707646,-1.4,6.76256313292354));
#12779=CARTESIAN_POINT('Origin',(1.23743686707646,-1.4,6.76256313292354));
#12780=CARTESIAN_POINT('',(1.01243686707646,-1.05,6.76256313292354));
#12781=CARTESIAN_POINT('',(1.01243686707646,-1.5,6.76256313292354));
#12782=CARTESIAN_POINT('Origin',(1.23743686707646,-1.05,6.76256313292354));
#12783=CARTESIAN_POINT('Origin',(0.,-1.4,8.));
#12784=CARTESIAN_POINT('',(-1.02,-1.05,8.));
#12785=CARTESIAN_POINT('Origin',(0.,-1.05,8.));
#12786=CARTESIAN_POINT('',(-1.02,-1.4,8.));
#12787=CARTESIAN_POINT('',(-1.02,-1.4,8.));
#12788=CARTESIAN_POINT('Origin',(0.,-1.4,8.));
#12789=CARTESIAN_POINT('Origin',(0.,-1.4,8.));
#12790=CARTESIAN_POINT('',(-2.2,-1.05,8.));
#12791=CARTESIAN_POINT('Origin',(0.,-1.05,8.));
#12792=CARTESIAN_POINT('',(-2.2,-1.4,8.));
#12793=CARTESIAN_POINT('',(-2.2,-1.4,8.));
#12794=CARTESIAN_POINT('Origin',(0.,-1.4,8.));
#12795=CARTESIAN_POINT('Origin',(0.,-1.05,8.));
#12796=CARTESIAN_POINT('Origin',(0.,-1.4,8.));
#12797=CARTESIAN_POINT('',(0.,0.,0.));
#12798=CARTESIAN_POINT('Origin',(-1.23743686707646,0.95,6.76256313292354));
#12799=CARTESIAN_POINT('',(-1.46243686707646,1.05,6.76256313292354));
#12800=CARTESIAN_POINT('Origin',(-1.23743686707646,1.05,6.76256313292354));
#12801=CARTESIAN_POINT('',(-1.46243686707646,1.4,6.76256313292354));
#12802=CARTESIAN_POINT('',(-1.46243686707646,0.95,6.76256313292354));
#12803=CARTESIAN_POINT('Origin',(-1.23743686707646,1.4,6.76256313292354));
#12804=CARTESIAN_POINT('Origin',(-1.23743686707646,0.95,9.23743686707646));
#12805=CARTESIAN_POINT('',(-1.46243686707646,1.05,9.23743686707646));
#12806=CARTESIAN_POINT('Origin',(-1.23743686707646,1.05,9.23743686707646));
#12807=CARTESIAN_POINT('',(-1.46243686707646,1.4,9.23743686707646));
#12808=CARTESIAN_POINT('',(-1.46243686707646,0.95,9.23743686707646));
#12809=CARTESIAN_POINT('Origin',(-1.23743686707646,1.4,9.23743686707646));
#12810=CARTESIAN_POINT('Origin',(1.23743686707646,0.95,9.23743686707646));
#12811=CARTESIAN_POINT('',(1.01243686707646,1.05,9.23743686707646));
#12812=CARTESIAN_POINT('Origin',(1.23743686707646,1.05,9.23743686707646));
#12813=CARTESIAN_POINT('',(1.01243686707646,1.4,9.23743686707646));
#12814=CARTESIAN_POINT('',(1.01243686707646,0.95,9.23743686707646));
#12815=CARTESIAN_POINT('Origin',(1.23743686707646,1.4,9.23743686707646));
#12816=CARTESIAN_POINT('Origin',(1.23743686707646,0.95,6.76256313292354));
#12817=CARTESIAN_POINT('',(1.01243686707646,1.05,6.76256313292354));
#12818=CARTESIAN_POINT('Origin',(1.23743686707646,1.05,6.76256313292354));
#12819=CARTESIAN_POINT('',(1.01243686707646,1.4,6.76256313292354));
#12820=CARTESIAN_POINT('',(1.01243686707646,0.95,6.76256313292354));
#12821=CARTESIAN_POINT('Origin',(1.23743686707646,1.4,6.76256313292354));
#12822=CARTESIAN_POINT('Origin',(0.,1.05,8.));
#12823=CARTESIAN_POINT('',(-1.02,1.4,8.));
#12824=CARTESIAN_POINT('Origin',(0.,1.4,8.));
#12825=CARTESIAN_POINT('',(-1.02,1.05,8.));
#12826=CARTESIAN_POINT('',(-1.02,1.05,8.));
#12827=CARTESIAN_POINT('Origin',(0.,1.05,8.));
#12828=CARTESIAN_POINT('Origin',(0.,1.05,8.));
#12829=CARTESIAN_POINT('',(-2.2,1.4,8.));
#12830=CARTESIAN_POINT('Origin',(0.,1.4,8.));
#12831=CARTESIAN_POINT('',(-2.2,1.05,8.));
#12832=CARTESIAN_POINT('',(-2.2,1.05,8.));
#12833=CARTESIAN_POINT('Origin',(0.,1.05,8.));
#12834=CARTESIAN_POINT('Origin',(0.,1.4,8.));
#12835=CARTESIAN_POINT('Origin',(0.,1.05,8.));
#12836=CARTESIAN_POINT('',(0.,0.,0.));
#12837=CARTESIAN_POINT('Origin',(20.,-0.15,8.));
#12838=CARTESIAN_POINT('',(18.98,0.15,8.));
#12839=CARTESIAN_POINT('Origin',(20.,0.15,8.));
#12840=CARTESIAN_POINT('',(18.98,-0.15,8.));
#12841=CARTESIAN_POINT('',(18.98,-0.15,8.));
#12842=CARTESIAN_POINT('Origin',(20.,-0.15,8.));
#12843=CARTESIAN_POINT('Origin',(20.,-0.15,8.));
#12844=CARTESIAN_POINT('',(18.51,0.15,8.));
#12845=CARTESIAN_POINT('Origin',(20.,0.15,8.));
#12846=CARTESIAN_POINT('',(18.51,-0.15,8.));
#12847=CARTESIAN_POINT('',(18.51,-0.15,8.));
#12848=CARTESIAN_POINT('Origin',(20.,-0.15,8.));
#12849=CARTESIAN_POINT('Origin',(20.,0.15,8.));
#12850=CARTESIAN_POINT('Origin',(20.,-0.15,8.));
#12851=CARTESIAN_POINT('',(0.,0.,0.));
#12852=CARTESIAN_POINT('Origin',(18.7625631329235,-1.5,6.76256313292354));
#12853=CARTESIAN_POINT('',(18.5375631329235,-1.4,6.76256313292354));
#12854=CARTESIAN_POINT('Origin',(18.7625631329235,-1.4,6.76256313292354));
#12855=CARTESIAN_POINT('',(18.5375631329235,-1.05,6.76256313292354));
#12856=CARTESIAN_POINT('',(18.5375631329235,-1.5,6.76256313292354));
#12857=CARTESIAN_POINT('Origin',(18.7625631329235,-1.05,6.76256313292354));
#12858=CARTESIAN_POINT('Origin',(18.7625631329235,-1.5,9.23743686707646));
#12859=CARTESIAN_POINT('',(18.5375631329235,-1.4,9.23743686707646));
#12860=CARTESIAN_POINT('Origin',(18.7625631329235,-1.4,9.23743686707646));
#12861=CARTESIAN_POINT('',(18.5375631329235,-1.05,9.23743686707646));
#12862=CARTESIAN_POINT('',(18.5375631329235,-1.5,9.23743686707646));
#12863=CARTESIAN_POINT('Origin',(18.7625631329235,-1.05,9.23743686707646));
#12864=CARTESIAN_POINT('Origin',(21.2374368670765,-1.5,9.23743686707646));
#12865=CARTESIAN_POINT('',(21.0124368670765,-1.4,9.23743686707646));
#12866=CARTESIAN_POINT('Origin',(21.2374368670765,-1.4,9.23743686707646));
#12867=CARTESIAN_POINT('',(21.0124368670765,-1.05,9.23743686707646));
#12868=CARTESIAN_POINT('',(21.0124368670765,-1.5,9.23743686707646));
#12869=CARTESIAN_POINT('Origin',(21.2374368670765,-1.05,9.23743686707646));
#12870=CARTESIAN_POINT('Origin',(21.2374368670765,-1.5,6.76256313292354));
#12871=CARTESIAN_POINT('',(21.0124368670765,-1.4,6.76256313292354));
#12872=CARTESIAN_POINT('Origin',(21.2374368670765,-1.4,6.76256313292354));
#12873=CARTESIAN_POINT('',(21.0124368670765,-1.05,6.76256313292354));
#12874=CARTESIAN_POINT('',(21.0124368670765,-1.5,6.76256313292354));
#12875=CARTESIAN_POINT('Origin',(21.2374368670765,-1.05,6.76256313292354));
#12876=CARTESIAN_POINT('Origin',(20.,-1.4,8.));
#12877=CARTESIAN_POINT('',(18.98,-1.05,8.));
#12878=CARTESIAN_POINT('Origin',(20.,-1.05,8.));
#12879=CARTESIAN_POINT('',(18.98,-1.4,8.));
#12880=CARTESIAN_POINT('',(18.98,-1.4,8.));
#12881=CARTESIAN_POINT('Origin',(20.,-1.4,8.));
#12882=CARTESIAN_POINT('Origin',(20.,-1.4,8.));
#12883=CARTESIAN_POINT('',(17.8,-1.05,8.));
#12884=CARTESIAN_POINT('Origin',(20.,-1.05,8.));
#12885=CARTESIAN_POINT('',(17.8,-1.4,8.));
#12886=CARTESIAN_POINT('',(17.8,-1.4,8.));
#12887=CARTESIAN_POINT('Origin',(20.,-1.4,8.));
#12888=CARTESIAN_POINT('Origin',(20.,-1.05,8.));
#12889=CARTESIAN_POINT('Origin',(20.,-1.4,8.));
#12890=CARTESIAN_POINT('',(0.,0.,0.));
#12891=CARTESIAN_POINT('Origin',(18.7625631329235,0.95,6.76256313292354));
#12892=CARTESIAN_POINT('',(18.5375631329235,1.05,6.76256313292354));
#12893=CARTESIAN_POINT('Origin',(18.7625631329235,1.05,6.76256313292354));
#12894=CARTESIAN_POINT('',(18.5375631329235,1.4,6.76256313292354));
#12895=CARTESIAN_POINT('',(18.5375631329235,0.95,6.76256313292354));
#12896=CARTESIAN_POINT('Origin',(18.7625631329235,1.4,6.76256313292354));
#12897=CARTESIAN_POINT('Origin',(18.7625631329235,0.95,9.23743686707646));
#12898=CARTESIAN_POINT('',(18.5375631329235,1.05,9.23743686707646));
#12899=CARTESIAN_POINT('Origin',(18.7625631329235,1.05,9.23743686707646));
#12900=CARTESIAN_POINT('',(18.5375631329235,1.4,9.23743686707646));
#12901=CARTESIAN_POINT('',(18.5375631329235,0.95,9.23743686707646));
#12902=CARTESIAN_POINT('Origin',(18.7625631329235,1.4,9.23743686707646));
#12903=CARTESIAN_POINT('Origin',(21.2374368670765,0.95,9.23743686707646));
#12904=CARTESIAN_POINT('',(21.0124368670765,1.05,9.23743686707646));
#12905=CARTESIAN_POINT('Origin',(21.2374368670765,1.05,9.23743686707646));
#12906=CARTESIAN_POINT('',(21.0124368670765,1.4,9.23743686707646));
#12907=CARTESIAN_POINT('',(21.0124368670765,0.95,9.23743686707646));
#12908=CARTESIAN_POINT('Origin',(21.2374368670765,1.4,9.23743686707646));
#12909=CARTESIAN_POINT('Origin',(21.2374368670765,0.95,6.76256313292354));
#12910=CARTESIAN_POINT('',(21.0124368670765,1.05,6.76256313292354));
#12911=CARTESIAN_POINT('Origin',(21.2374368670765,1.05,6.76256313292354));
#12912=CARTESIAN_POINT('',(21.0124368670765,1.4,6.76256313292354));
#12913=CARTESIAN_POINT('',(21.0124368670765,0.95,6.76256313292354));
#12914=CARTESIAN_POINT('Origin',(21.2374368670765,1.4,6.76256313292354));
#12915=CARTESIAN_POINT('Origin',(20.,1.05,8.));
#12916=CARTESIAN_POINT('',(18.98,1.4,8.));
#12917=CARTESIAN_POINT('Origin',(20.,1.4,8.));
#12918=CARTESIAN_POINT('',(18.98,1.05,8.));
#12919=CARTESIAN_POINT('',(18.98,1.05,8.));
#12920=CARTESIAN_POINT('Origin',(20.,1.05,8.));
#12921=CARTESIAN_POINT('Origin',(20.,1.05,8.));
#12922=CARTESIAN_POINT('',(17.8,1.4,8.));
#12923=CARTESIAN_POINT('Origin',(20.,1.4,8.));
#12924=CARTESIAN_POINT('',(17.8,1.05,8.));
#12925=CARTESIAN_POINT('',(17.8,1.05,8.));
#12926=CARTESIAN_POINT('Origin',(20.,1.05,8.));
#12927=CARTESIAN_POINT('Origin',(20.,1.4,8.));
#12928=CARTESIAN_POINT('Origin',(20.,1.05,8.));
#12929=CARTESIAN_POINT('',(0.,0.,0.));
#12930=CARTESIAN_POINT('Origin',(3.4,-3.4,8.));
#12931=CARTESIAN_POINT('',(3.5,-3.4,8.07));
#12932=CARTESIAN_POINT('Origin',(3.5,-3.4,8.));
#12933=CARTESIAN_POINT('',(4.5,-3.4,8.07));
#12934=CARTESIAN_POINT('',(3.4,-3.4,8.07));
#12935=CARTESIAN_POINT('Origin',(4.5,-3.4,8.));
#12936=CARTESIAN_POINT('Origin',(4.5,-1.05,7.5));
#12937=CARTESIAN_POINT('',(4.5,-1.05,7.5));
#12938=CARTESIAN_POINT('',(3.5,-1.05,7.5));
#12939=CARTESIAN_POINT('',(4.5,-1.05,7.5));
#12940=CARTESIAN_POINT('',(3.5,-1.05,8.5));
#12941=CARTESIAN_POINT('',(3.5,-1.05,7.5));
#12942=CARTESIAN_POINT('',(4.5,-1.05,8.5));
#12943=CARTESIAN_POINT('',(4.5,-1.05,8.5));
#12944=CARTESIAN_POINT('',(4.5,-1.05,7.5));
#12945=CARTESIAN_POINT('Origin',(4.5,-3.8,7.5));
#12946=CARTESIAN_POINT('',(4.5,-3.8,7.5));
#12947=CARTESIAN_POINT('',(4.5,-3.8,7.5));
#12948=CARTESIAN_POINT('',(4.5,-3.8,8.5));
#12949=CARTESIAN_POINT('',(4.5,-3.8,8.5));
#12950=CARTESIAN_POINT('',(4.5,-3.8,7.5));
#12951=CARTESIAN_POINT('Origin',(3.5,-3.8,7.5));
#12952=CARTESIAN_POINT('',(3.5,-3.8,7.5));
#12953=CARTESIAN_POINT('',(3.5,-3.8,7.5));
#12954=CARTESIAN_POINT('',(3.5,-3.8,8.5));
#12955=CARTESIAN_POINT('',(3.5,-3.8,8.5));
#12956=CARTESIAN_POINT('',(3.5,-3.8,7.5));
#12957=CARTESIAN_POINT('Origin',(3.5,-1.05,7.5));
#12958=CARTESIAN_POINT('',(3.5,-1.05,7.5));
#12959=CARTESIAN_POINT('',(3.5,-1.05,8.5));
#12960=CARTESIAN_POINT('Origin',(4.,-2.425,8.5));
#12961=CARTESIAN_POINT('Origin',(4.,-2.425,7.5));
#12962=CARTESIAN_POINT('',(0.,0.,0.));
#12963=CARTESIAN_POINT('',(0.,0.,0.));
#12964=CARTESIAN_POINT('Origin',(18.7625631329235,-1.15,12.7625631329235));
#12965=CARTESIAN_POINT('',(18.5975631329235,-1.05,12.7625631329235));
#12966=CARTESIAN_POINT('Origin',(18.7625631329235,-1.05,12.7625631329235));
#12967=CARTESIAN_POINT('',(18.5975631329235,1.05,12.7625631329235));
#12968=CARTESIAN_POINT('',(18.5975631329235,-1.15,12.7625631329235));
#12969=CARTESIAN_POINT('Origin',(18.7625631329235,1.05,12.7625631329235));
#12970=CARTESIAN_POINT('Origin',(18.7625631329235,-1.15,15.2374368670765));
#12971=CARTESIAN_POINT('',(18.5975631329235,-1.05,15.2374368670765));
#12972=CARTESIAN_POINT('Origin',(18.7625631329235,-1.05,15.2374368670765));
#12973=CARTESIAN_POINT('',(18.5975631329235,1.05,15.2374368670765));
#12974=CARTESIAN_POINT('',(18.5975631329235,-1.15,15.2374368670765));
#12975=CARTESIAN_POINT('Origin',(18.7625631329235,1.05,15.2374368670765));
#12976=CARTESIAN_POINT('Origin',(21.2374368670765,-1.15,15.2374368670765));
#12977=CARTESIAN_POINT('',(21.0724368670765,-1.05,15.2374368670765));
#12978=CARTESIAN_POINT('Origin',(21.2374368670765,-1.05,15.2374368670765));
#12979=CARTESIAN_POINT('',(21.0724368670765,1.05,15.2374368670765));
#12980=CARTESIAN_POINT('',(21.0724368670765,-1.15,15.2374368670765));
#12981=CARTESIAN_POINT('Origin',(21.2374368670765,1.05,15.2374368670765));
#12982=CARTESIAN_POINT('Origin',(21.2374368670765,-1.15,12.7625631329235));
#12983=CARTESIAN_POINT('',(21.0724368670765,-1.05,12.7625631329235));
#12984=CARTESIAN_POINT('Origin',(21.2374368670765,-1.05,12.7625631329235));
#12985=CARTESIAN_POINT('',(21.0724368670765,1.05,12.7625631329235));
#12986=CARTESIAN_POINT('',(21.0724368670765,-1.15,12.7625631329235));
#12987=CARTESIAN_POINT('Origin',(21.2374368670765,1.05,12.7625631329235));
#12988=CARTESIAN_POINT('Origin',(-1.23743686707646,-1.15,12.7625631329235));
#12989=CARTESIAN_POINT('',(-1.40243686707646,-1.05,12.7625631329235));
#12990=CARTESIAN_POINT('Origin',(-1.23743686707646,-1.05,12.7625631329235));
#12991=CARTESIAN_POINT('',(-1.40243686707646,1.05,12.7625631329235));
#12992=CARTESIAN_POINT('',(-1.40243686707646,-1.15,12.7625631329235));
#12993=CARTESIAN_POINT('Origin',(-1.23743686707646,1.05,12.7625631329235));
#12994=CARTESIAN_POINT('Origin',(-1.23743686707646,-1.15,15.2374368670765));
#12995=CARTESIAN_POINT('',(-1.40243686707646,-1.05,15.2374368670765));
#12996=CARTESIAN_POINT('Origin',(-1.23743686707646,-1.05,15.2374368670765));
#12997=CARTESIAN_POINT('',(-1.40243686707646,1.05,15.2374368670765));
#12998=CARTESIAN_POINT('',(-1.40243686707646,-1.15,15.2374368670765));
#12999=CARTESIAN_POINT('Origin',(-1.23743686707646,1.05,15.2374368670765));
#13000=CARTESIAN_POINT('Origin',(1.23743686707646,-1.15,15.2374368670765));
#13001=CARTESIAN_POINT('',(1.07243686707646,-1.05,15.2374368670765));
#13002=CARTESIAN_POINT('Origin',(1.23743686707646,-1.05,15.2374368670765));
#13003=CARTESIAN_POINT('',(1.07243686707646,1.05,15.2374368670765));
#13004=CARTESIAN_POINT('',(1.07243686707646,-1.15,15.2374368670765));
#13005=CARTESIAN_POINT('Origin',(1.23743686707646,1.05,15.2374368670765));
#13006=CARTESIAN_POINT('Origin',(1.23743686707646,-1.15,12.7625631329235));
#13007=CARTESIAN_POINT('',(1.07243686707646,-1.05,12.7625631329235));
#13008=CARTESIAN_POINT('Origin',(1.23743686707646,-1.05,12.7625631329235));
#13009=CARTESIAN_POINT('',(1.07243686707646,1.05,12.7625631329235));
#13010=CARTESIAN_POINT('',(1.07243686707646,-1.15,12.7625631329235));
#13011=CARTESIAN_POINT('Origin',(1.23743686707646,1.05,12.7625631329235));
#13012=CARTESIAN_POINT('Origin',(0.,-1.15,14.));
#13013=CARTESIAN_POINT('',(-1.5,-1.05,14.));
#13014=CARTESIAN_POINT('Origin',(0.,-1.05,14.));
#13015=CARTESIAN_POINT('',(-1.5,1.05,14.));
#13016=CARTESIAN_POINT('',(-1.5,-1.15,14.));
#13017=CARTESIAN_POINT('Origin',(0.,1.05,14.));
#13018=CARTESIAN_POINT('Origin',(20.,-1.15,14.));
#13019=CARTESIAN_POINT('',(18.5,-1.05,14.));
#13020=CARTESIAN_POINT('Origin',(20.,-1.05,14.));
#13021=CARTESIAN_POINT('',(18.5,1.05,14.));
#13022=CARTESIAN_POINT('',(18.5,-1.15,14.));
#13023=CARTESIAN_POINT('Origin',(20.,1.05,14.));
#13024=CARTESIAN_POINT('Origin',(20.,-1.05,14.));
#13025=CARTESIAN_POINT('',(17.9506098468081,1.05,13.2));
#13026=CARTESIAN_POINT('',(17.9506098468081,-1.05,13.2));
#13027=CARTESIAN_POINT('',(17.9506098468081,-1.05,13.2));
#13028=CARTESIAN_POINT('',(17.9506098468081,1.05,14.8));
#13029=CARTESIAN_POINT('Origin',(20.,1.05,14.));
#13030=CARTESIAN_POINT('',(17.9506098468081,-1.05,14.8));
#13031=CARTESIAN_POINT('',(17.9506098468081,-1.05,14.8));
#13032=CARTESIAN_POINT('Origin',(20.,-1.05,14.));
#13033=CARTESIAN_POINT('Origin',(20.,-1.05,13.2));
#13034=CARTESIAN_POINT('',(2.04939015319192,-1.05,13.2));
#13035=CARTESIAN_POINT('',(0.,-1.05,13.2));
#13036=CARTESIAN_POINT('',(2.04939015319192,1.05,13.2));
#13037=CARTESIAN_POINT('',(2.04939015319192,-1.05,13.2));
#13038=CARTESIAN_POINT('',(0.,1.05,13.2));
#13039=CARTESIAN_POINT('Origin',(0.,-1.05,14.));
#13040=CARTESIAN_POINT('',(2.04939015319192,-1.05,14.8));
#13041=CARTESIAN_POINT('',(20.,-1.05,14.8));
#13042=CARTESIAN_POINT('Origin',(0.,-1.05,14.));
#13043=CARTESIAN_POINT('Origin',(0.,-1.05,14.8));
#13044=CARTESIAN_POINT('',(2.04939015319192,1.05,14.8));
#13045=CARTESIAN_POINT('',(20.,1.05,14.8));
#13046=CARTESIAN_POINT('',(2.04939015319192,-1.05,14.8));
#13047=CARTESIAN_POINT('Origin',(0.,-1.05,14.));
#13048=CARTESIAN_POINT('Origin',(0.,1.05,14.));
#13049=CARTESIAN_POINT('Origin',(0.,1.05,14.));
#13050=CARTESIAN_POINT('',(0.,0.,0.));
#13051=CARTESIAN_POINT('Origin',(0.,-0.15,14.));
#13052=CARTESIAN_POINT('',(-1.02,0.15,14.));
#13053=CARTESIAN_POINT('Origin',(0.,0.15,14.));
#13054=CARTESIAN_POINT('',(-1.02,-0.15,14.));
#13055=CARTESIAN_POINT('',(-1.02,-0.15,14.));
#13056=CARTESIAN_POINT('Origin',(0.,-0.15,14.));
#13057=CARTESIAN_POINT('Origin',(0.,-0.15,14.));
#13058=CARTESIAN_POINT('',(-1.49,0.15,14.));
#13059=CARTESIAN_POINT('Origin',(0.,0.15,14.));
#13060=CARTESIAN_POINT('',(-1.49,-0.15,14.));
#13061=CARTESIAN_POINT('',(-1.49,-0.15,14.));
#13062=CARTESIAN_POINT('Origin',(0.,-0.15,14.));
#13063=CARTESIAN_POINT('Origin',(0.,0.15,14.));
#13064=CARTESIAN_POINT('Origin',(0.,-0.15,14.));
#13065=CARTESIAN_POINT('',(0.,0.,0.));
#13066=CARTESIAN_POINT('Origin',(-1.23743686707646,-1.5,12.7625631329235));
#13067=CARTESIAN_POINT('',(-1.46243686707646,-1.4,12.7625631329235));
#13068=CARTESIAN_POINT('Origin',(-1.23743686707646,-1.4,12.7625631329235));
#13069=CARTESIAN_POINT('',(-1.46243686707646,-1.05,12.7625631329235));
#13070=CARTESIAN_POINT('',(-1.46243686707646,-1.5,12.7625631329235));
#13071=CARTESIAN_POINT('Origin',(-1.23743686707646,-1.05,12.7625631329235));
#13072=CARTESIAN_POINT('Origin',(-1.23743686707646,-1.5,15.2374368670765));
#13073=CARTESIAN_POINT('',(-1.46243686707646,-1.4,15.2374368670765));
#13074=CARTESIAN_POINT('Origin',(-1.23743686707646,-1.4,15.2374368670765));
#13075=CARTESIAN_POINT('',(-1.46243686707646,-1.05,15.2374368670765));
#13076=CARTESIAN_POINT('',(-1.46243686707646,-1.5,15.2374368670765));
#13077=CARTESIAN_POINT('Origin',(-1.23743686707646,-1.05,15.2374368670765));
#13078=CARTESIAN_POINT('Origin',(1.23743686707646,-1.5,15.2374368670765));
#13079=CARTESIAN_POINT('',(1.01243686707646,-1.4,15.2374368670765));
#13080=CARTESIAN_POINT('Origin',(1.23743686707646,-1.4,15.2374368670765));
#13081=CARTESIAN_POINT('',(1.01243686707646,-1.05,15.2374368670765));
#13082=CARTESIAN_POINT('',(1.01243686707646,-1.5,15.2374368670765));
#13083=CARTESIAN_POINT('Origin',(1.23743686707646,-1.05,15.2374368670765));
#13084=CARTESIAN_POINT('Origin',(1.23743686707646,-1.5,12.7625631329235));
#13085=CARTESIAN_POINT('',(1.01243686707646,-1.4,12.7625631329235));
#13086=CARTESIAN_POINT('Origin',(1.23743686707646,-1.4,12.7625631329235));
#13087=CARTESIAN_POINT('',(1.01243686707646,-1.05,12.7625631329235));
#13088=CARTESIAN_POINT('',(1.01243686707646,-1.5,12.7625631329235));
#13089=CARTESIAN_POINT('Origin',(1.23743686707646,-1.05,12.7625631329235));
#13090=CARTESIAN_POINT('Origin',(0.,-1.4,14.));
#13091=CARTESIAN_POINT('',(-1.02,-1.05,14.));
#13092=CARTESIAN_POINT('Origin',(0.,-1.05,14.));
#13093=CARTESIAN_POINT('',(-1.02,-1.4,14.));
#13094=CARTESIAN_POINT('',(-1.02,-1.4,14.));
#13095=CARTESIAN_POINT('Origin',(0.,-1.4,14.));
#13096=CARTESIAN_POINT('Origin',(0.,-1.4,14.));
#13097=CARTESIAN_POINT('',(-2.2,-1.05,14.));
#13098=CARTESIAN_POINT('Origin',(0.,-1.05,14.));
#13099=CARTESIAN_POINT('',(-2.2,-1.4,14.));
#13100=CARTESIAN_POINT('',(-2.2,-1.4,14.));
#13101=CARTESIAN_POINT('Origin',(0.,-1.4,14.));
#13102=CARTESIAN_POINT('Origin',(0.,-1.05,14.));
#13103=CARTESIAN_POINT('Origin',(0.,-1.4,14.));
#13104=CARTESIAN_POINT('',(0.,0.,0.));
#13105=CARTESIAN_POINT('Origin',(-1.23743686707646,0.95,12.7625631329235));
#13106=CARTESIAN_POINT('',(-1.46243686707646,1.05,12.7625631329235));
#13107=CARTESIAN_POINT('Origin',(-1.23743686707646,1.05,12.7625631329235));
#13108=CARTESIAN_POINT('',(-1.46243686707646,1.4,12.7625631329235));
#13109=CARTESIAN_POINT('',(-1.46243686707646,0.95,12.7625631329235));
#13110=CARTESIAN_POINT('Origin',(-1.23743686707646,1.4,12.7625631329235));
#13111=CARTESIAN_POINT('Origin',(-1.23743686707646,0.95,15.2374368670765));
#13112=CARTESIAN_POINT('',(-1.46243686707646,1.05,15.2374368670765));
#13113=CARTESIAN_POINT('Origin',(-1.23743686707646,1.05,15.2374368670765));
#13114=CARTESIAN_POINT('',(-1.46243686707646,1.4,15.2374368670765));
#13115=CARTESIAN_POINT('',(-1.46243686707646,0.95,15.2374368670765));
#13116=CARTESIAN_POINT('Origin',(-1.23743686707646,1.4,15.2374368670765));
#13117=CARTESIAN_POINT('Origin',(1.23743686707646,0.95,15.2374368670765));
#13118=CARTESIAN_POINT('',(1.01243686707646,1.05,15.2374368670765));
#13119=CARTESIAN_POINT('Origin',(1.23743686707646,1.05,15.2374368670765));
#13120=CARTESIAN_POINT('',(1.01243686707646,1.4,15.2374368670765));
#13121=CARTESIAN_POINT('',(1.01243686707646,0.95,15.2374368670765));
#13122=CARTESIAN_POINT('Origin',(1.23743686707646,1.4,15.2374368670765));
#13123=CARTESIAN_POINT('Origin',(1.23743686707646,0.95,12.7625631329235));
#13124=CARTESIAN_POINT('',(1.01243686707646,1.05,12.7625631329235));
#13125=CARTESIAN_POINT('Origin',(1.23743686707646,1.05,12.7625631329235));
#13126=CARTESIAN_POINT('',(1.01243686707646,1.4,12.7625631329235));
#13127=CARTESIAN_POINT('',(1.01243686707646,0.95,12.7625631329235));
#13128=CARTESIAN_POINT('Origin',(1.23743686707646,1.4,12.7625631329235));
#13129=CARTESIAN_POINT('Origin',(0.,1.05,14.));
#13130=CARTESIAN_POINT('',(-1.02,1.4,14.));
#13131=CARTESIAN_POINT('Origin',(0.,1.4,14.));
#13132=CARTESIAN_POINT('',(-1.02,1.05,14.));
#13133=CARTESIAN_POINT('',(-1.02,1.05,14.));
#13134=CARTESIAN_POINT('Origin',(0.,1.05,14.));
#13135=CARTESIAN_POINT('Origin',(0.,1.05,14.));
#13136=CARTESIAN_POINT('',(-2.2,1.4,14.));
#13137=CARTESIAN_POINT('Origin',(0.,1.4,14.));
#13138=CARTESIAN_POINT('',(-2.2,1.05,14.));
#13139=CARTESIAN_POINT('',(-2.2,1.05,14.));
#13140=CARTESIAN_POINT('Origin',(0.,1.05,14.));
#13141=CARTESIAN_POINT('Origin',(0.,1.4,14.));
#13142=CARTESIAN_POINT('Origin',(0.,1.05,14.));
#13143=CARTESIAN_POINT('',(0.,0.,0.));
#13144=CARTESIAN_POINT('Origin',(20.,-0.15,14.));
#13145=CARTESIAN_POINT('',(18.98,0.15,14.));
#13146=CARTESIAN_POINT('Origin',(20.,0.15,14.));
#13147=CARTESIAN_POINT('',(18.98,-0.15,14.));
#13148=CARTESIAN_POINT('',(18.98,-0.15,14.));
#13149=CARTESIAN_POINT('Origin',(20.,-0.15,14.));
#13150=CARTESIAN_POINT('Origin',(20.,-0.15,14.));
#13151=CARTESIAN_POINT('',(18.51,0.15,14.));
#13152=CARTESIAN_POINT('Origin',(20.,0.15,14.));
#13153=CARTESIAN_POINT('',(18.51,-0.15,14.));
#13154=CARTESIAN_POINT('',(18.51,-0.15,14.));
#13155=CARTESIAN_POINT('Origin',(20.,-0.15,14.));
#13156=CARTESIAN_POINT('Origin',(20.,0.15,14.));
#13157=CARTESIAN_POINT('Origin',(20.,-0.15,14.));
#13158=CARTESIAN_POINT('',(0.,0.,0.));
#13159=CARTESIAN_POINT('Origin',(18.7625631329235,-1.5,12.7625631329235));
#13160=CARTESIAN_POINT('',(18.5375631329235,-1.4,12.7625631329235));
#13161=CARTESIAN_POINT('Origin',(18.7625631329235,-1.4,12.7625631329235));
#13162=CARTESIAN_POINT('',(18.5375631329235,-1.05,12.7625631329235));
#13163=CARTESIAN_POINT('',(18.5375631329235,-1.5,12.7625631329235));
#13164=CARTESIAN_POINT('Origin',(18.7625631329235,-1.05,12.7625631329235));
#13165=CARTESIAN_POINT('Origin',(18.7625631329235,-1.5,15.2374368670765));
#13166=CARTESIAN_POINT('',(18.5375631329235,-1.4,15.2374368670765));
#13167=CARTESIAN_POINT('Origin',(18.7625631329235,-1.4,15.2374368670765));
#13168=CARTESIAN_POINT('',(18.5375631329235,-1.05,15.2374368670765));
#13169=CARTESIAN_POINT('',(18.5375631329235,-1.5,15.2374368670765));
#13170=CARTESIAN_POINT('Origin',(18.7625631329235,-1.05,15.2374368670765));
#13171=CARTESIAN_POINT('Origin',(21.2374368670765,-1.5,15.2374368670765));
#13172=CARTESIAN_POINT('',(21.0124368670765,-1.4,15.2374368670765));
#13173=CARTESIAN_POINT('Origin',(21.2374368670765,-1.4,15.2374368670765));
#13174=CARTESIAN_POINT('',(21.0124368670765,-1.05,15.2374368670765));
#13175=CARTESIAN_POINT('',(21.0124368670765,-1.5,15.2374368670765));
#13176=CARTESIAN_POINT('Origin',(21.2374368670765,-1.05,15.2374368670765));
#13177=CARTESIAN_POINT('Origin',(21.2374368670765,-1.5,12.7625631329235));
#13178=CARTESIAN_POINT('',(21.0124368670765,-1.4,12.7625631329235));
#13179=CARTESIAN_POINT('Origin',(21.2374368670765,-1.4,12.7625631329235));
#13180=CARTESIAN_POINT('',(21.0124368670765,-1.05,12.7625631329235));
#13181=CARTESIAN_POINT('',(21.0124368670765,-1.5,12.7625631329235));
#13182=CARTESIAN_POINT('Origin',(21.2374368670765,-1.05,12.7625631329235));
#13183=CARTESIAN_POINT('Origin',(20.,-1.4,14.));
#13184=CARTESIAN_POINT('',(18.98,-1.05,14.));
#13185=CARTESIAN_POINT('Origin',(20.,-1.05,14.));
#13186=CARTESIAN_POINT('',(18.98,-1.4,14.));
#13187=CARTESIAN_POINT('',(18.98,-1.4,14.));
#13188=CARTESIAN_POINT('Origin',(20.,-1.4,14.));
#13189=CARTESIAN_POINT('Origin',(20.,-1.4,14.));
#13190=CARTESIAN_POINT('',(17.8,-1.05,14.));
#13191=CARTESIAN_POINT('Origin',(20.,-1.05,14.));
#13192=CARTESIAN_POINT('',(17.8,-1.4,14.));
#13193=CARTESIAN_POINT('',(17.8,-1.4,14.));
#13194=CARTESIAN_POINT('Origin',(20.,-1.4,14.));
#13195=CARTESIAN_POINT('Origin',(20.,-1.05,14.));
#13196=CARTESIAN_POINT('Origin',(20.,-1.4,14.));
#13197=CARTESIAN_POINT('',(0.,0.,0.));
#13198=CARTESIAN_POINT('Origin',(18.7625631329235,0.95,12.7625631329235));
#13199=CARTESIAN_POINT('',(18.5375631329235,1.05,12.7625631329235));
#13200=CARTESIAN_POINT('Origin',(18.7625631329235,1.05,12.7625631329235));
#13201=CARTESIAN_POINT('',(18.5375631329235,1.4,12.7625631329235));
#13202=CARTESIAN_POINT('',(18.5375631329235,0.95,12.7625631329235));
#13203=CARTESIAN_POINT('Origin',(18.7625631329235,1.4,12.7625631329235));
#13204=CARTESIAN_POINT('Origin',(18.7625631329235,0.95,15.2374368670765));
#13205=CARTESIAN_POINT('',(18.5375631329235,1.05,15.2374368670765));
#13206=CARTESIAN_POINT('Origin',(18.7625631329235,1.05,15.2374368670765));
#13207=CARTESIAN_POINT('',(18.5375631329235,1.4,15.2374368670765));
#13208=CARTESIAN_POINT('',(18.5375631329235,0.95,15.2374368670765));
#13209=CARTESIAN_POINT('Origin',(18.7625631329235,1.4,15.2374368670765));
#13210=CARTESIAN_POINT('Origin',(21.2374368670765,0.95,15.2374368670765));
#13211=CARTESIAN_POINT('',(21.0124368670765,1.05,15.2374368670765));
#13212=CARTESIAN_POINT('Origin',(21.2374368670765,1.05,15.2374368670765));
#13213=CARTESIAN_POINT('',(21.0124368670765,1.4,15.2374368670765));
#13214=CARTESIAN_POINT('',(21.0124368670765,0.95,15.2374368670765));
#13215=CARTESIAN_POINT('Origin',(21.2374368670765,1.4,15.2374368670765));
#13216=CARTESIAN_POINT('Origin',(21.2374368670765,0.95,12.7625631329235));
#13217=CARTESIAN_POINT('',(21.0124368670765,1.05,12.7625631329235));
#13218=CARTESIAN_POINT('Origin',(21.2374368670765,1.05,12.7625631329235));
#13219=CARTESIAN_POINT('',(21.0124368670765,1.4,12.7625631329235));
#13220=CARTESIAN_POINT('',(21.0124368670765,0.95,12.7625631329235));
#13221=CARTESIAN_POINT('Origin',(21.2374368670765,1.4,12.7625631329235));
#13222=CARTESIAN_POINT('Origin',(20.,1.05,14.));
#13223=CARTESIAN_POINT('',(18.98,1.4,14.));
#13224=CARTESIAN_POINT('Origin',(20.,1.4,14.));
#13225=CARTESIAN_POINT('',(18.98,1.05,14.));
#13226=CARTESIAN_POINT('',(18.98,1.05,14.));
#13227=CARTESIAN_POINT('Origin',(20.,1.05,14.));
#13228=CARTESIAN_POINT('Origin',(20.,1.05,14.));
#13229=CARTESIAN_POINT('',(17.8,1.4,14.));
#13230=CARTESIAN_POINT('Origin',(20.,1.4,14.));
#13231=CARTESIAN_POINT('',(17.8,1.05,14.));
#13232=CARTESIAN_POINT('',(17.8,1.05,14.));
#13233=CARTESIAN_POINT('Origin',(20.,1.05,14.));
#13234=CARTESIAN_POINT('Origin',(20.,1.4,14.));
#13235=CARTESIAN_POINT('Origin',(20.,1.05,14.));
#13236=CARTESIAN_POINT('',(0.,0.,0.));
#13237=CARTESIAN_POINT('',(0.,0.,0.));
#13238=CARTESIAN_POINT('Origin',(0.,0.,0.));
#13239=CARTESIAN_POINT('',(-0.976185,-0.246528389340863,-1.19548183562566E-16));
#13240=CARTESIAN_POINT('',(-1.19548183562566E-16,-0.246528389340863,0.976185));
#13241=CARTESIAN_POINT('Origin',(0.,-0.246528389340863,0.));
#13242=CARTESIAN_POINT('Origin',(0.,-0.246528389340863,0.));
#13243=CARTESIAN_POINT('',(-1.19548183562566E-16,0.246528389340863,0.976185));
#13244=CARTESIAN_POINT('Origin',(-1.22464679914735E-16,0.,1.));
#13245=CARTESIAN_POINT('',(-0.976185,0.246528389340863,1.19548183562566E-16));
#13246=CARTESIAN_POINT('Origin',(0.,0.246528389340863,0.));
#13247=CARTESIAN_POINT('Origin',(0.,0.246528389340863,0.));
#13248=CARTESIAN_POINT('Origin',(0.,0.,0.));
#13249=CARTESIAN_POINT('',(-0.976185,0.45,-1.19548183562566E-16));
#13250=CARTESIAN_POINT('',(-0.976185,0.,-1.19548183562566E-16));
#13251=CARTESIAN_POINT('Origin',(0.,0.45,0.));
#13252=CARTESIAN_POINT('Origin',(0.,0.,0.));
#13253=CARTESIAN_POINT('',(-0.5,-0.39,-6.12323399573677E-17));
#13254=CARTESIAN_POINT('Origin',(0.,-0.39,0.));
#13255=CARTESIAN_POINT('',(-0.5,0.39,-6.12323399573677E-17));
#13256=CARTESIAN_POINT('',(-0.5,0.,-6.12323399573677E-17));
#13257=CARTESIAN_POINT('Origin',(0.,0.39,0.));
#13258=CARTESIAN_POINT('Origin',(0.,0.42,0.));
#13259=CARTESIAN_POINT('',(-0.56,0.45,-6.85802207522518E-17));
#13260=CARTESIAN_POINT('',(-0.53,0.42,-6.49062803548097E-17));
#13261=CARTESIAN_POINT('Origin',(0.,0.45,0.));
#13262=CARTESIAN_POINT('Origin',(0.976185,0.45,0.));
#13263=CARTESIAN_POINT('Origin',(0.,0.,0.));
#13264=CARTESIAN_POINT('',(-0.976185,-0.45,-1.19548183562566E-16));
#13265=CARTESIAN_POINT('Origin',(0.,-0.45,0.));
#13266=CARTESIAN_POINT('',(-0.976185,0.,-1.19548183562566E-16));
#13267=CARTESIAN_POINT('Origin',(0.56,-0.45,0.));
#13268=CARTESIAN_POINT('',(-0.56,-0.45,-6.85802207522518E-17));
#13269=CARTESIAN_POINT('Origin',(0.,-0.45,0.));
#13270=CARTESIAN_POINT('Origin',(0.,-0.42,0.));
#13271=CARTESIAN_POINT('',(-0.53,-0.42,-6.49062803548097E-17));
#13272=CARTESIAN_POINT('',(0.,0.,0.));
#13273=CARTESIAN_POINT('Origin',(0.,0.,0.));
#13274=CARTESIAN_POINT('',(-1.023815,0.246528389340863,-1.25381176266905E-16));
#13275=CARTESIAN_POINT('',(-1.25381176266905E-16,0.246528389340863,1.023815));
#13276=CARTESIAN_POINT('Origin',(0.,0.246528389340863,0.));
#13277=CARTESIAN_POINT('Origin',(0.,0.246528389340863,0.));
#13278=CARTESIAN_POINT('',(-1.25381176266905E-16,-0.246528389340863,1.023815));
#13279=CARTESIAN_POINT('Origin',(-1.22464679914735E-16,0.,1.));
#13280=CARTESIAN_POINT('',(-1.023815,-0.246528389340863,1.25381176266905E-16));
#13281=CARTESIAN_POINT('Origin',(0.,-0.246528389340863,0.));
#13282=CARTESIAN_POINT('Origin',(0.,-0.246528389340863,0.));
#13283=CARTESIAN_POINT('Origin',(0.,0.,0.));
#13284=CARTESIAN_POINT('',(-1.023815,-0.45,-1.25381176266905E-16));
#13285=CARTESIAN_POINT('Origin',(0.,-0.45,0.));
#13286=CARTESIAN_POINT('',(-1.023815,0.,-1.25381176266905E-16));
#13287=CARTESIAN_POINT('Origin',(1.44,0.45,0.));
#13288=CARTESIAN_POINT('',(-1.44,0.45,-1.76349139077219E-16));
#13289=CARTESIAN_POINT('Origin',(0.,0.45,0.));
#13290=CARTESIAN_POINT('',(-1.023815,0.45,-1.25381176266905E-16));
#13291=CARTESIAN_POINT('Origin',(0.,0.45,0.));
#13292=CARTESIAN_POINT('Origin',(0.,0.42,0.));
#13293=CARTESIAN_POINT('',(-1.5,0.39,-1.83697019872103E-16));
#13294=CARTESIAN_POINT('Origin',(0.,0.39,0.));
#13295=CARTESIAN_POINT('',(-1.47,0.42,-1.80023079474661E-16));
#13296=CARTESIAN_POINT('Origin',(0.,0.,0.));
#13297=CARTESIAN_POINT('',(-1.5,-0.39,-1.83697019872103E-16));
#13298=CARTESIAN_POINT('Origin',(0.,-0.39,0.));
#13299=CARTESIAN_POINT('',(-1.5,0.,-1.83697019872103E-16));
#13300=CARTESIAN_POINT('Origin',(0.,-0.42,0.));
#13301=CARTESIAN_POINT('',(-1.44,-0.45,-1.76349139077219E-16));
#13302=CARTESIAN_POINT('Origin',(0.,-0.45,0.));
#13303=CARTESIAN_POINT('',(-1.47,-0.42,-1.80023079474661E-16));
#13304=CARTESIAN_POINT('Origin',(1.023815,-0.45,0.));
#13305=CARTESIAN_POINT('Origin',(0.,0.,0.));
#13306=CARTESIAN_POINT('',(-1.023815,0.,-1.25381176266905E-16));
#13307=CARTESIAN_POINT('',(0.,0.,0.));
#13308=CARTESIAN_POINT('Origin',(1.,0.,0.));
#13309=CARTESIAN_POINT('',(1.,-1.78583896120461E-33,0.23815));
#13310=CARTESIAN_POINT('',(1.,-1.78583896120461E-33,-0.23815));
#13311=CARTESIAN_POINT('Origin',(1.,0.,0.));
#13312=CARTESIAN_POINT('Origin',(0.707106781186548,0.,-0.707106781186547));
#13313=CARTESIAN_POINT('',(0.875504261126124,-1.78583896120461E-33,-0.538709301246971));
#13314=CARTESIAN_POINT('',(0.538709301246971,-1.78583896120461E-33,-0.875504261126124));
#13315=CARTESIAN_POINT('Origin',(0.707106781186548,0.,-0.707106781186547));
#13316=CARTESIAN_POINT('Origin',(6.12323399573677E-17,0.,-1.));
#13317=CARTESIAN_POINT('',(0.23815,-1.78583896120461E-33,-1.));
#13318=CARTESIAN_POINT('',(-0.23815,-1.78583896120461E-33,-1.));
#13319=CARTESIAN_POINT('Origin',(6.12323399573677E-17,0.,-1.));
#13320=CARTESIAN_POINT('Origin',(-0.707106781186547,0.,-0.707106781186548));
#13321=CARTESIAN_POINT('',(-0.538709301246971,-1.78583896120461E-33,-0.875504261126124));
#13322=CARTESIAN_POINT('',(-0.875504261126124,-1.78583896120461E-33,-0.538709301246971));
#13323=CARTESIAN_POINT('Origin',(-0.707106781186547,0.,-0.707106781186548));
#13324=CARTESIAN_POINT('Origin',(-1.,0.,-1.22464679914735E-16));
#13325=CARTESIAN_POINT('',(-1.,-1.78583896120461E-33,-0.23815));
#13326=CARTESIAN_POINT('',(-1.,-1.78583896120461E-33,0.23815));
#13327=CARTESIAN_POINT('Origin',(-1.,0.,-1.22464679914735E-16));
#13328=CARTESIAN_POINT('Origin',(-0.707106781186548,0.,0.707106781186547));
#13329=CARTESIAN_POINT('',(-0.875504261126124,-7.94881478324376E-33,0.538709301246971));
#13330=CARTESIAN_POINT('',(-0.538709301246971,4.37713686083455E-33,0.875504261126124));
#13331=CARTESIAN_POINT('Origin',(-0.707106781186548,0.,0.707106781186547));
#13332=CARTESIAN_POINT('Origin',(-1.83697019872103E-16,0.,1.));
#13333=CARTESIAN_POINT('',(-0.23815,-1.78583896120461E-33,1.));
#13334=CARTESIAN_POINT('',(0.23815,-1.78583896120461E-33,1.));
#13335=CARTESIAN_POINT('Origin',(-1.83697019872103E-16,0.,1.));
#13336=CARTESIAN_POINT('Origin',(0.707106781186547,0.,0.707106781186548));
#13337=CARTESIAN_POINT('',(0.538709301246971,-4.86732687222419E-33,0.875504261126124));
#13338=CARTESIAN_POINT('',(0.875504261126124,1.29564894981497E-33,0.538709301246971));
#13339=CARTESIAN_POINT('Origin',(0.707106781186547,0.,0.707106781186548));
#13340=CARTESIAN_POINT('',(0.,0.,0.));
#13341=CARTESIAN_POINT('Origin',(0.707106781186547,0.,0.707106781186548));
#13342=CARTESIAN_POINT('',(0.504455939115715,-0.04763,0.841298510752802));
#13343=CARTESIAN_POINT('',(0.841298510752802,-0.04763,0.504455939115715));
#13344=CARTESIAN_POINT('Ctrl Pts',(0.504455939115715,-0.04763,0.841298510752802));
#13345=CARTESIAN_POINT('Ctrl Pts',(0.508899795931835,-0.0740444353928835,
0.838633903678357));
#13346=CARTESIAN_POINT('Ctrl Pts',(0.517157748491652,-0.0999305678883309,
0.833661031856294));
#13347=CARTESIAN_POINT('Ctrl Pts',(0.537715343527944,-0.142345102874864,
0.820511285096538));
#13348=CARTESIAN_POINT('Ctrl Pts',(0.548874290046456,-0.159766064500479,
0.813159949759));
#13349=CARTESIAN_POINT('Ctrl Pts',(0.573915184558107,-0.190326085855194,
0.795684265985089));
#13350=CARTESIAN_POINT('Ctrl Pts',(0.587792702767295,-0.203463743702801,
0.78555112003688));
#13351=CARTESIAN_POINT('Ctrl Pts',(0.615966552324775,-0.224161999508995,
0.763642258217233));
#13352=CARTESIAN_POINT('Ctrl Pts',(0.631684198665438,-0.232861760990032,
0.750785745543687));
#13353=CARTESIAN_POINT('Ctrl Pts',(0.663382628119203,-0.244251601209411,
0.722929908501543));
#13354=CARTESIAN_POINT('Ctrl Pts',(0.679352081686668,-0.246942143572133,
0.707917883896095));
#13355=CARTESIAN_POINT('Ctrl Pts',(0.707917883896095,-0.246942143572133,
0.679352081686668));
#13356=CARTESIAN_POINT('Ctrl Pts',(0.722929908501543,-0.244251601209411,
0.663382628119203));
#13357=CARTESIAN_POINT('Ctrl Pts',(0.750785745543687,-0.232861760990032,
0.631684198665439));
#13358=CARTESIAN_POINT('Ctrl Pts',(0.763642258217232,-0.224161999508995,
0.615966552324775));
#13359=CARTESIAN_POINT('Ctrl Pts',(0.78555112003688,-0.203463743702801,
0.587792702767295));
#13360=CARTESIAN_POINT('Ctrl Pts',(0.795684265985088,-0.190326085855194,
0.573915184558108));
#13361=CARTESIAN_POINT('Ctrl Pts',(0.813159949759,-0.15976606450048,0.548874290046456));
#13362=CARTESIAN_POINT('Ctrl Pts',(0.820511285096538,-0.142345102874864,
0.537715343527944));
#13363=CARTESIAN_POINT('Ctrl Pts',(0.833661031856294,-0.099930567888331,
0.517157748491653));
#13364=CARTESIAN_POINT('Ctrl Pts',(0.838633903678357,-0.0740444353928835,
0.508899795931835));
#13365=CARTESIAN_POINT('Ctrl Pts',(0.841298510752801,-0.0476299999999999,
0.504455939115715));
#13366=CARTESIAN_POINT('',(0.528110872004958,-0.04763,0.871530771444223));
#13367=CARTESIAN_POINT('Origin',(0.707106781186547,-0.04763,0.707106781186548));
#13368=CARTESIAN_POINT('',(0.871530771444223,-0.04763,0.528110872004959));
#13369=CARTESIAN_POINT('Ctrl Pts',(0.871530771444223,-0.0476300000000001,
0.528110872004958));
#13370=CARTESIAN_POINT('Ctrl Pts',(0.87014664509073,-0.0609922781173483,
0.530395067942936));
#13371=CARTESIAN_POINT('Ctrl Pts',(0.868149331745851,-0.0742967091364493,
0.533674141594226));
#13372=CARTESIAN_POINT('Ctrl Pts',(0.85981294420286,-0.115492077056649,
0.54708917182331));
#13373=CARTESIAN_POINT('Ctrl Pts',(0.850993704737257,-0.141695629206859,
0.560922177770136));
#13374=CARTESIAN_POINT('Ctrl Pts',(0.830754510485543,-0.181890537957859,
0.590422647829571));
#13375=CARTESIAN_POINT('Ctrl Pts',(0.816896541396381,-0.201072148666545,
0.609616703125488));
#13376=CARTESIAN_POINT('Ctrl Pts',(0.792310597819928,-0.223955109275652,
0.641117951819998));
#13377=CARTESIAN_POINT('Ctrl Pts',(0.779109323683612,-0.232742381310829,
0.657208095763053));
#13378=CARTESIAN_POINT('Ctrl Pts',(0.750552691816206,-0.244234834628584,
0.68964083160521));
#13379=CARTESIAN_POINT('Ctrl Pts',(0.735185187071673,-0.246942143572133,
0.705971972091755));
#13380=CARTESIAN_POINT('Ctrl Pts',(0.705971972091754,-0.246942143572133,
0.735185187071673));
#13381=CARTESIAN_POINT('Ctrl Pts',(0.689640831605209,-0.244234834628584,
0.750552691816206));
#13382=CARTESIAN_POINT('Ctrl Pts',(0.657208095763052,-0.232742381310829,
0.779109323683612));
#13383=CARTESIAN_POINT('Ctrl Pts',(0.641117951819998,-0.223955109275652,
0.792310597819928));
#13384=CARTESIAN_POINT('Ctrl Pts',(0.609616703125487,-0.201072148666545,
0.816896541396382));
#13385=CARTESIAN_POINT('Ctrl Pts',(0.590422647829571,-0.181890537957858,
0.830754510485544));
#13386=CARTESIAN_POINT('Ctrl Pts',(0.560922177770135,-0.141695629206858,
0.850993704737257));
#13387=CARTESIAN_POINT('Ctrl Pts',(0.547089171823309,-0.115492077056649,
0.859812944202861));
#13388=CARTESIAN_POINT('Ctrl Pts',(0.533674141594226,-0.0742967091364491,
0.868149331745852));
#13389=CARTESIAN_POINT('Ctrl Pts',(0.530395067942936,-0.0609922781173483,
0.870146645090731));
#13390=CARTESIAN_POINT('Ctrl Pts',(0.528110872004958,-0.0476300000000001,
0.871530771444223));
#13391=CARTESIAN_POINT('Origin',(0.707106781186547,-0.04763,0.707106781186548));
#13392=CARTESIAN_POINT('Origin',(0.,-0.166705,0.));
#13393=CARTESIAN_POINT('',(0.242834539687906,-0.04763,0.989696097314));
#13394=CARTESIAN_POINT('Origin',(0.,-0.04763,0.));
#13395=CARTESIAN_POINT('',(-0.242834539687907,-0.04763,0.989696097314));
#13396=CARTESIAN_POINT('Ctrl Pts',(0.242834539687906,-0.04763,0.989696097314));
#13397=CARTESIAN_POINT('Ctrl Pts',(0.24024064412003,-0.0609922781173483,
0.990332542620729));
#13398=CARTESIAN_POINT('Ctrl Pts',(0.236509675094874,-0.0742967091364492,
0.991238884025248));
#13399=CARTESIAN_POINT('Ctrl Pts',(0.221129100087819,-0.115492077056649,
0.994830026707808));
#13400=CARTESIAN_POINT('Ctrl Pts',(0.205111543747588,-0.141695629206859,
0.998375294985966));
#13401=CARTESIAN_POINT('Ctrl Pts',(0.169940289819232,-0.181890537957859,
1.00492400591205));
#13402=CARTESIAN_POINT('Ctrl Pts',(0.1465689792446,-0.201072148666545,1.00869718865384));
#13403=CARTESIAN_POINT('Ctrl Pts',(0.106909345252087,-0.223955109275652,
1.01358704779679));
#13404=CARTESIAN_POINT('Ctrl Pts',(0.0861971848975941,-0.232742381310829,
1.0156297872271));
#13405=CARTESIAN_POINT('Ctrl Pts',(0.0430711894098822,-0.244234834628584,
1.01837060663223));
#13406=CARTESIAN_POINT('Ctrl Pts',(0.0206568624125605,-0.246942143572133,
1.019052));
#13407=CARTESIAN_POINT('Ctrl Pts',(-0.0206568624125608,-0.246942143572133,
1.019052));
#13408=CARTESIAN_POINT('Ctrl Pts',(-0.0430711894098825,-0.244234834628584,
1.01837060663223));
#13409=CARTESIAN_POINT('Ctrl Pts',(-0.0861971848975943,-0.232742381310829,
1.0156297872271));
#13410=CARTESIAN_POINT('Ctrl Pts',(-0.106909345252088,-0.223955109275652,
1.01358704779679));
#13411=CARTESIAN_POINT('Ctrl Pts',(-0.1465689792446,-0.201072148666545,
1.00869718865384));
#13412=CARTESIAN_POINT('Ctrl Pts',(-0.169940289819232,-0.181890537957859,
1.00492400591205));
#13413=CARTESIAN_POINT('Ctrl Pts',(-0.205111543747588,-0.141695629206859,
0.998375294985966));
#13414=CARTESIAN_POINT('Ctrl Pts',(-0.221129100087819,-0.115492077056649,
0.994830026707808));
#13415=CARTESIAN_POINT('Ctrl Pts',(-0.236509675094875,-0.0742967091364493,
0.991238884025248));
#13416=CARTESIAN_POINT('Ctrl Pts',(-0.24024064412003,-0.0609922781173483,
0.990332542620729));
#13417=CARTESIAN_POINT('Ctrl Pts',(-0.242834539687907,-0.04763,0.989696097314));
#13418=CARTESIAN_POINT('',(-0.528110872004959,-0.04763,0.871530771444223));
#13419=CARTESIAN_POINT('Origin',(0.,-0.04763,0.));
#13420=CARTESIAN_POINT('',(-0.871530771444223,-0.04763,0.528110872004958));
#13421=CARTESIAN_POINT('Ctrl Pts',(-0.528110872004958,-0.0476300000000001,
0.871530771444223));
#13422=CARTESIAN_POINT('Ctrl Pts',(-0.530395067942936,-0.0609922781173484,
0.87014664509073));
#13423=CARTESIAN_POINT('Ctrl Pts',(-0.533674141594226,-0.0742967091364493,
0.868149331745851));
#13424=CARTESIAN_POINT('Ctrl Pts',(-0.54708917182331,-0.115492077056649,
0.85981294420286));
#13425=CARTESIAN_POINT('Ctrl Pts',(-0.560922177770136,-0.141695629206859,
0.850993704737257));
#13426=CARTESIAN_POINT('Ctrl Pts',(-0.590422647829571,-0.181890537957859,
0.830754510485543));
#13427=CARTESIAN_POINT('Ctrl Pts',(-0.609616703125488,-0.201072148666545,
0.816896541396381));
#13428=CARTESIAN_POINT('Ctrl Pts',(-0.641117951819998,-0.223955109275652,
0.792310597819928));
#13429=CARTESIAN_POINT('Ctrl Pts',(-0.657208095763053,-0.232742381310829,
0.779109323683611));
#13430=CARTESIAN_POINT('Ctrl Pts',(-0.68964083160521,-0.244234834628584,
0.750552691816205));
#13431=CARTESIAN_POINT('Ctrl Pts',(-0.705971972091755,-0.246942143572133,
0.735185187071673));
#13432=CARTESIAN_POINT('Ctrl Pts',(-0.735185187071673,-0.246942143572133,
0.705971972091754));
#13433=CARTESIAN_POINT('Ctrl Pts',(-0.750552691816206,-0.244234834628584,
0.689640831605209));
#13434=CARTESIAN_POINT('Ctrl Pts',(-0.779109323683612,-0.232742381310829,
0.657208095763052));
#13435=CARTESIAN_POINT('Ctrl Pts',(-0.792310597819928,-0.223955109275652,
0.641117951819998));
#13436=CARTESIAN_POINT('Ctrl Pts',(-0.816896541396382,-0.201072148666545,
0.609616703125487));
#13437=CARTESIAN_POINT('Ctrl Pts',(-0.830754510485544,-0.181890537957858,
0.590422647829571));
#13438=CARTESIAN_POINT('Ctrl Pts',(-0.850993704737257,-0.141695629206858,
0.560922177770135));
#13439=CARTESIAN_POINT('Ctrl Pts',(-0.859812944202861,-0.115492077056649,
0.547089171823309));
#13440=CARTESIAN_POINT('Ctrl Pts',(-0.868149331745852,-0.0742967091364491,
0.533674141594226));
#13441=CARTESIAN_POINT('Ctrl Pts',(-0.870146645090731,-0.0609922781173483,
0.530395067942936));
#13442=CARTESIAN_POINT('Ctrl Pts',(-0.871530771444223,-0.04763,0.528110872004958));
#13443=CARTESIAN_POINT('',(-0.989696097314,-0.04763,0.242834539687906));
#13444=CARTESIAN_POINT('Origin',(0.,-0.04763,0.));
#13445=CARTESIAN_POINT('',(-1.019052,-0.246942143572133,1.248489836334E-16));
#13446=CARTESIAN_POINT('Ctrl Pts',(-0.989696097314,-0.04763,0.242834539687906));
#13447=CARTESIAN_POINT('Ctrl Pts',(-0.990332542620729,-0.0609922781173483,
0.24024064412003));
#13448=CARTESIAN_POINT('Ctrl Pts',(-0.991238884025248,-0.0742967091364492,
0.236509675094874));
#13449=CARTESIAN_POINT('Ctrl Pts',(-0.994830026707808,-0.115492077056649,
0.221129100087819));
#13450=CARTESIAN_POINT('Ctrl Pts',(-0.998375294985966,-0.141695629206859,
0.205111543747588));
#13451=CARTESIAN_POINT('Ctrl Pts',(-1.00492400591205,-0.181890537957859,
0.169940289819232));
#13452=CARTESIAN_POINT('Ctrl Pts',(-1.00869718865384,-0.201072148666545,
0.1465689792446));
#13453=CARTESIAN_POINT('Ctrl Pts',(-1.01358704779679,-0.223955109275652,
0.106909345252088));
#13454=CARTESIAN_POINT('Ctrl Pts',(-1.0156297872271,-0.232742381310829,
0.0861971848975944));
#13455=CARTESIAN_POINT('Ctrl Pts',(-1.01837060663223,-0.244234834628584,
0.0430711894098825));
#13456=CARTESIAN_POINT('Ctrl Pts',(-1.019052,-0.246942143572133,0.0206568624125608));
#13457=CARTESIAN_POINT('Ctrl Pts',(-1.019052,-0.246942143572133,1.2490009027033E-16));
#13458=CARTESIAN_POINT('',(-1.019052,-0.28578,1.24797876996471E-16));
#13459=CARTESIAN_POINT('',(-1.019052,-0.166705,1.24797876996471E-16));
#13460=CARTESIAN_POINT('Origin',(0.,-0.28578,0.));
#13461=CARTESIAN_POINT('',(-0.989696097314,-0.04763,-0.242834539687906));
#13462=CARTESIAN_POINT('Ctrl Pts',(-1.019052,-0.246942143572133,1.2490009027033E-16));
#13463=CARTESIAN_POINT('Ctrl Pts',(-1.019052,-0.246942143572133,-0.0206568624125605));
#13464=CARTESIAN_POINT('Ctrl Pts',(-1.01837060663223,-0.244234834628584,
-0.0430711894098822));
#13465=CARTESIAN_POINT('Ctrl Pts',(-1.0156297872271,-0.232742381310829,
-0.0861971848975941));
#13466=CARTESIAN_POINT('Ctrl Pts',(-1.01358704779679,-0.223955109275652,
-0.106909345252087));
#13467=CARTESIAN_POINT('Ctrl Pts',(-1.00869718865384,-0.201072148666546,
-0.1465689792446));
#13468=CARTESIAN_POINT('Ctrl Pts',(-1.00492400591205,-0.181890537957859,
-0.169940289819232));
#13469=CARTESIAN_POINT('Ctrl Pts',(-0.998375294985966,-0.141695629206859,
-0.205111543747588));
#13470=CARTESIAN_POINT('Ctrl Pts',(-0.994830026707808,-0.11549207705665,
-0.221129100087819));
#13471=CARTESIAN_POINT('Ctrl Pts',(-0.991238884025248,-0.0742967091364495,
-0.236509675094874));
#13472=CARTESIAN_POINT('Ctrl Pts',(-0.990332542620729,-0.0609922781173484,
-0.24024064412003));
#13473=CARTESIAN_POINT('Ctrl Pts',(-0.989696097314,-0.0476300000000001,
-0.242834539687907));
#13474=CARTESIAN_POINT('',(-0.871530771444223,-0.04763,-0.528110872004958));
#13475=CARTESIAN_POINT('Origin',(0.,-0.04763,0.));
#13476=CARTESIAN_POINT('',(-0.528110872004958,-0.04763,-0.871530771444223));
#13477=CARTESIAN_POINT('Ctrl Pts',(-0.871530771444223,-0.0476300000000001,
-0.528110872004958));
#13478=CARTESIAN_POINT('Ctrl Pts',(-0.87014664509073,-0.0609922781173484,
-0.530395067942936));
#13479=CARTESIAN_POINT('Ctrl Pts',(-0.868149331745851,-0.0742967091364494,
-0.533674141594226));
#13480=CARTESIAN_POINT('Ctrl Pts',(-0.85981294420286,-0.115492077056649,
-0.54708917182331));
#13481=CARTESIAN_POINT('Ctrl Pts',(-0.850993704737257,-0.141695629206859,
-0.560922177770136));
#13482=CARTESIAN_POINT('Ctrl Pts',(-0.830754510485543,-0.181890537957859,
-0.590422647829571));
#13483=CARTESIAN_POINT('Ctrl Pts',(-0.816896541396381,-0.201072148666546,
-0.609616703125488));
#13484=CARTESIAN_POINT('Ctrl Pts',(-0.792310597819928,-0.223955109275652,
-0.641117951819999));
#13485=CARTESIAN_POINT('Ctrl Pts',(-0.779109323683611,-0.232742381310829,
-0.657208095763053));
#13486=CARTESIAN_POINT('Ctrl Pts',(-0.750552691816205,-0.244234834628584,
-0.68964083160521));
#13487=CARTESIAN_POINT('Ctrl Pts',(-0.735185187071673,-0.246942143572133,
-0.705971972091755));
#13488=CARTESIAN_POINT('Ctrl Pts',(-0.705971972091754,-0.246942143572133,
-0.735185187071673));
#13489=CARTESIAN_POINT('Ctrl Pts',(-0.68964083160521,-0.244234834628584,
-0.750552691816206));
#13490=CARTESIAN_POINT('Ctrl Pts',(-0.657208095763052,-0.232742381310829,
-0.779109323683612));
#13491=CARTESIAN_POINT('Ctrl Pts',(-0.641117951819998,-0.223955109275652,
-0.792310597819928));
#13492=CARTESIAN_POINT('Ctrl Pts',(-0.609616703125488,-0.201072148666545,
-0.816896541396381));
#13493=CARTESIAN_POINT('Ctrl Pts',(-0.590422647829571,-0.181890537957859,
-0.830754510485543));
#13494=CARTESIAN_POINT('Ctrl Pts',(-0.560922177770136,-0.141695629206859,
-0.850993704737257));
#13495=CARTESIAN_POINT('Ctrl Pts',(-0.54708917182331,-0.115492077056649,
-0.85981294420286));
#13496=CARTESIAN_POINT('Ctrl Pts',(-0.533674141594226,-0.0742967091364494,
-0.868149331745852));
#13497=CARTESIAN_POINT('Ctrl Pts',(-0.530395067942936,-0.0609922781173484,
-0.870146645090731));
#13498=CARTESIAN_POINT('Ctrl Pts',(-0.528110872004958,-0.0476300000000001,
-0.871530771444223));
#13499=CARTESIAN_POINT('',(-0.242834539687906,-0.04763,-0.989696097314));
#13500=CARTESIAN_POINT('Origin',(0.,-0.04763,0.));
#13501=CARTESIAN_POINT('',(0.242834539687906,-0.04763,-0.989696097314));
#13502=CARTESIAN_POINT('Ctrl Pts',(-0.242834539687907,-0.04763,-0.989696097314));
#13503=CARTESIAN_POINT('Ctrl Pts',(-0.24024064412003,-0.0609922781173483,
-0.990332542620729));
#13504=CARTESIAN_POINT('Ctrl Pts',(-0.236509675094874,-0.0742967091364493,
-0.991238884025248));
#13505=CARTESIAN_POINT('Ctrl Pts',(-0.221129100087819,-0.115492077056649,
-0.994830026707808));
#13506=CARTESIAN_POINT('Ctrl Pts',(-0.205111543747588,-0.141695629206859,
-0.998375294985966));
#13507=CARTESIAN_POINT('Ctrl Pts',(-0.169940289819232,-0.181890537957859,
-1.00492400591205));
#13508=CARTESIAN_POINT('Ctrl Pts',(-0.1465689792446,-0.201072148666545,
-1.00869718865384));
#13509=CARTESIAN_POINT('Ctrl Pts',(-0.106909345252087,-0.223955109275652,
-1.01358704779679));
#13510=CARTESIAN_POINT('Ctrl Pts',(-0.0861971848975942,-0.232742381310829,
-1.0156297872271));
#13511=CARTESIAN_POINT('Ctrl Pts',(-0.0430711894098823,-0.244234834628584,
-1.01837060663223));
#13512=CARTESIAN_POINT('Ctrl Pts',(-0.0206568624125606,-0.246942143572133,
-1.019052));
#13513=CARTESIAN_POINT('Ctrl Pts',(0.0206568624125607,-0.246942143572133,
-1.019052));
#13514=CARTESIAN_POINT('Ctrl Pts',(0.0430711894098824,-0.244234834628584,
-1.01837060663223));
#13515=CARTESIAN_POINT('Ctrl Pts',(0.0861971848975943,-0.232742381310829,
-1.0156297872271));
#13516=CARTESIAN_POINT('Ctrl Pts',(0.106909345252088,-0.223955109275652,
-1.01358704779679));
#13517=CARTESIAN_POINT('Ctrl Pts',(0.1465689792446,-0.201072148666545,-1.00869718865384));
#13518=CARTESIAN_POINT('Ctrl Pts',(0.169940289819232,-0.181890537957859,
-1.00492400591205));
#13519=CARTESIAN_POINT('Ctrl Pts',(0.205111543747588,-0.141695629206859,
-0.998375294985966));
#13520=CARTESIAN_POINT('Ctrl Pts',(0.221129100087819,-0.115492077056649,
-0.994830026707808));
#13521=CARTESIAN_POINT('Ctrl Pts',(0.236509675094874,-0.0742967091364493,
-0.991238884025248));
#13522=CARTESIAN_POINT('Ctrl Pts',(0.24024064412003,-0.0609922781173484,
-0.990332542620729));
#13523=CARTESIAN_POINT('Ctrl Pts',(0.242834539687907,-0.04763,-0.989696097314));
#13524=CARTESIAN_POINT('',(0.528110872004958,-0.04763,-0.871530771444223));
#13525=CARTESIAN_POINT('Origin',(0.,-0.04763,0.));
#13526=CARTESIAN_POINT('',(0.871530771444223,-0.04763,-0.528110872004958));
#13527=CARTESIAN_POINT('Ctrl Pts',(0.528110872004958,-0.0476300000000001,
-0.871530771444223));
#13528=CARTESIAN_POINT('Ctrl Pts',(0.530395067942936,-0.0609922781173484,
-0.870146645090731));
#13529=CARTESIAN_POINT('Ctrl Pts',(0.533674141594226,-0.0742967091364493,
-0.868149331745851));
#13530=CARTESIAN_POINT('Ctrl Pts',(0.54708917182331,-0.115492077056649,
-0.85981294420286));
#13531=CARTESIAN_POINT('Ctrl Pts',(0.560922177770136,-0.141695629206859,
-0.850993704737257));
#13532=CARTESIAN_POINT('Ctrl Pts',(0.590422647829571,-0.181890537957859,
-0.830754510485543));
#13533=CARTESIAN_POINT('Ctrl Pts',(0.609616703125488,-0.201072148666545,
-0.816896541396381));
#13534=CARTESIAN_POINT('Ctrl Pts',(0.641117951819998,-0.223955109275652,
-0.792310597819928));
#13535=CARTESIAN_POINT('Ctrl Pts',(0.657208095763053,-0.232742381310829,
-0.779109323683612));
#13536=CARTESIAN_POINT('Ctrl Pts',(0.68964083160521,-0.244234834628584,
-0.750552691816206));
#13537=CARTESIAN_POINT('Ctrl Pts',(0.705971972091755,-0.246942143572133,
-0.735185187071673));
#13538=CARTESIAN_POINT('Ctrl Pts',(0.735185187071673,-0.246942143572133,
-0.705971972091754));
#13539=CARTESIAN_POINT('Ctrl Pts',(0.750552691816206,-0.244234834628584,
-0.68964083160521));
#13540=CARTESIAN_POINT('Ctrl Pts',(0.779109323683612,-0.232742381310829,
-0.657208095763053));
#13541=CARTESIAN_POINT('Ctrl Pts',(0.792310597819928,-0.223955109275652,
-0.641117951819998));
#13542=CARTESIAN_POINT('Ctrl Pts',(0.816896541396381,-0.201072148666545,
-0.609616703125488));
#13543=CARTESIAN_POINT('Ctrl Pts',(0.830754510485543,-0.181890537957859,
-0.590422647829571));
#13544=CARTESIAN_POINT('Ctrl Pts',(0.850993704737257,-0.141695629206859,
-0.560922177770136));
#13545=CARTESIAN_POINT('Ctrl Pts',(0.85981294420286,-0.115492077056649,
-0.54708917182331));
#13546=CARTESIAN_POINT('Ctrl Pts',(0.868149331745851,-0.0742967091364493,
-0.533674141594226));
#13547=CARTESIAN_POINT('Ctrl Pts',(0.870146645090731,-0.0609922781173484,
-0.530395067942936));
#13548=CARTESIAN_POINT('Ctrl Pts',(0.871530771444223,-0.0476300000000001,
-0.528110872004958));
#13549=CARTESIAN_POINT('',(0.989696097314,-0.04763,-0.242834539687906));
#13550=CARTESIAN_POINT('Origin',(0.,-0.04763,0.));
#13551=CARTESIAN_POINT('',(0.989696097314,-0.04763,0.242834539687906));
#13552=CARTESIAN_POINT('Ctrl Pts',(0.989696097314,-0.04763,-0.242834539687907));
#13553=CARTESIAN_POINT('Ctrl Pts',(0.990332542620729,-0.0609922781173483,
-0.24024064412003));
#13554=CARTESIAN_POINT('Ctrl Pts',(0.991238884025248,-0.0742967091364493,
-0.236509675094874));
#13555=CARTESIAN_POINT('Ctrl Pts',(0.994830026707808,-0.115492077056649,
-0.221129100087819));
#13556=CARTESIAN_POINT('Ctrl Pts',(0.998375294985966,-0.141695629206859,
-0.205111543747588));
#13557=CARTESIAN_POINT('Ctrl Pts',(1.00492400591205,-0.181890537957859,
-0.169940289819232));
#13558=CARTESIAN_POINT('Ctrl Pts',(1.00869718865384,-0.201072148666545,
-0.1465689792446));
#13559=CARTESIAN_POINT('Ctrl Pts',(1.01358704779679,-0.223955109275652,
-0.106909345252087));
#13560=CARTESIAN_POINT('Ctrl Pts',(1.0156297872271,-0.232742381310829,-0.0861971848975942));
#13561=CARTESIAN_POINT('Ctrl Pts',(1.01837060663223,-0.244234834628584,
-0.0430711894098823));
#13562=CARTESIAN_POINT('Ctrl Pts',(1.019052,-0.246942143572133,-0.0206568624125607));
#13563=CARTESIAN_POINT('Ctrl Pts',(1.019052,-0.246942143572133,0.0206568624125607));
#13564=CARTESIAN_POINT('Ctrl Pts',(1.01837060663223,-0.244234834628584,
0.0430711894098823));
#13565=CARTESIAN_POINT('Ctrl Pts',(1.0156297872271,-0.232742381310829,0.0861971848975942));
#13566=CARTESIAN_POINT('Ctrl Pts',(1.01358704779679,-0.223955109275652,
0.106909345252087));
#13567=CARTESIAN_POINT('Ctrl Pts',(1.00869718865384,-0.201072148666545,
0.1465689792446));
#13568=CARTESIAN_POINT('Ctrl Pts',(1.00492400591205,-0.181890537957859,
0.169940289819232));
#13569=CARTESIAN_POINT('Ctrl Pts',(0.998375294985966,-0.141695629206859,
0.205111543747588));
#13570=CARTESIAN_POINT('Ctrl Pts',(0.994830026707808,-0.115492077056649,
0.221129100087819));
#13571=CARTESIAN_POINT('Ctrl Pts',(0.991238884025248,-0.0742967091364492,
0.236509675094874));
#13572=CARTESIAN_POINT('Ctrl Pts',(0.990332542620729,-0.0609922781173483,
0.24024064412003));
#13573=CARTESIAN_POINT('Ctrl Pts',(0.989696097314,-0.04763,0.242834539687907));
#13574=CARTESIAN_POINT('Origin',(0.,-0.04763,0.));
#13575=CARTESIAN_POINT('Origin',(0.,-0.04763,0.));
#13576=CARTESIAN_POINT('',(0.238183666596899,-0.04763,0.951592097314));
#13577=CARTESIAN_POINT('Origin',(0.,-0.04763,0.));
#13578=CARTESIAN_POINT('Origin',(-1.94289029309402E-16,-0.04763,1.));
#13579=CARTESIAN_POINT('Origin',(-1.94289029309402E-16,0.,1.));
#13580=CARTESIAN_POINT('',(-0.2381836665969,-0.04763,0.951592097314));
#13581=CARTESIAN_POINT('Ctrl Pts',(-0.238183666596899,-0.0476299999999999,
0.951592097314));
#13582=CARTESIAN_POINT('Ctrl Pts',(-0.233157223576062,-0.0740444353928835,
0.952850216871763));
#13583=CARTESIAN_POINT('Ctrl Pts',(-0.223801617934946,-0.0999305678883309,
0.955173119738174));
#13584=CARTESIAN_POINT('Ctrl Pts',(-0.199966927975188,-0.142345102874864,
0.960411259488514));
#13585=CARTESIAN_POINT('Ctrl Pts',(-0.1868781821531,-0.159766064500479,
0.963103647174702));
#13586=CARTESIAN_POINT('Ctrl Pts',(-0.15681442133453,-0.190326085855194,
0.968453058988463));
#13587=CARTESIAN_POINT('Ctrl Pts',(-0.139836317888043,-0.203463743702801,
0.971100730005489));
#13588=CARTESIAN_POINT('Ctrl Pts',(-0.104422493053067,-0.224161999508995,
0.975530745318961));
#13589=CARTESIAN_POINT('Ctrl Pts',(-0.0842175114474176,-0.232861760990032,
0.977553872336861));
#13590=CARTESIAN_POINT('Ctrl Pts',(-0.0421062857595701,-0.244251601209411,
0.980270995488453));
#13591=CARTESIAN_POINT('Ctrl Pts',(-0.0201990724523197,-0.246942143572133,
0.980948));
#13592=CARTESIAN_POINT('Ctrl Pts',(0.020199072452319,-0.246942143572133,
0.980948));
#13593=CARTESIAN_POINT('Ctrl Pts',(0.0421062857595694,-0.244251601209411,
0.980270995488454));
#13594=CARTESIAN_POINT('Ctrl Pts',(0.0842175114474169,-0.232861760990032,
0.977553872336861));
#13595=CARTESIAN_POINT('Ctrl Pts',(0.104422493053067,-0.224161999508995,
0.975530745318961));
#13596=CARTESIAN_POINT('Ctrl Pts',(0.139836317888042,-0.203463743702801,
0.971100730005489));
#13597=CARTESIAN_POINT('Ctrl Pts',(0.15681442133453,-0.190326085855194,
0.968453058988463));
#13598=CARTESIAN_POINT('Ctrl Pts',(0.1868781821531,-0.15976606450048,0.963103647174702));
#13599=CARTESIAN_POINT('Ctrl Pts',(0.199966927975188,-0.142345102874864,
0.960411259488514));
#13600=CARTESIAN_POINT('Ctrl Pts',(0.223801617934945,-0.0999305678883309,
0.955173119738174));
#13601=CARTESIAN_POINT('Ctrl Pts',(0.233157223576061,-0.0740444353928835,
0.952850216871763));
#13602=CARTESIAN_POINT('Ctrl Pts',(0.238183666596899,-0.0476299999999999,
0.951592097314));
#13603=CARTESIAN_POINT('Origin',(-1.94289029309402E-16,-0.04763,1.));
#13604=CARTESIAN_POINT('Origin',(0.,-0.04763,0.));
#13605=CARTESIAN_POINT('',(-0.504455939115715,-0.04763,0.841298510752802));
#13606=CARTESIAN_POINT('Origin',(0.,-0.04763,0.));
#13607=CARTESIAN_POINT('Origin',(-0.707106781186548,-0.04763,0.707106781186547));
#13608=CARTESIAN_POINT('Origin',(-0.707106781186548,0.,0.707106781186547));
#13609=CARTESIAN_POINT('',(-0.841298510752802,-0.04763,0.504455939115715));
#13610=CARTESIAN_POINT('Ctrl Pts',(-0.841298510752802,-0.04763,0.504455939115715));
#13611=CARTESIAN_POINT('Ctrl Pts',(-0.838633903678357,-0.0740444353928835,
0.508899795931835));
#13612=CARTESIAN_POINT('Ctrl Pts',(-0.833661031856294,-0.0999305678883309,
0.517157748491652));
#13613=CARTESIAN_POINT('Ctrl Pts',(-0.820511285096538,-0.142345102874864,
0.537715343527944));
#13614=CARTESIAN_POINT('Ctrl Pts',(-0.813159949759,-0.159766064500479,0.548874290046456));
#13615=CARTESIAN_POINT('Ctrl Pts',(-0.795684265985089,-0.190326085855194,
0.573915184558107));
#13616=CARTESIAN_POINT('Ctrl Pts',(-0.78555112003688,-0.203463743702801,
0.587792702767295));
#13617=CARTESIAN_POINT('Ctrl Pts',(-0.763642258217233,-0.224161999508995,
0.615966552324775));
#13618=CARTESIAN_POINT('Ctrl Pts',(-0.750785745543687,-0.232861760990032,
0.631684198665438));
#13619=CARTESIAN_POINT('Ctrl Pts',(-0.722929908501543,-0.244251601209411,
0.663382628119203));
#13620=CARTESIAN_POINT('Ctrl Pts',(-0.707917883896095,-0.246942143572133,
0.679352081686668));
#13621=CARTESIAN_POINT('Ctrl Pts',(-0.679352081686668,-0.246942143572133,
0.707917883896095));
#13622=CARTESIAN_POINT('Ctrl Pts',(-0.663382628119203,-0.244251601209411,
0.722929908501544));
#13623=CARTESIAN_POINT('Ctrl Pts',(-0.631684198665438,-0.232861760990031,
0.750785745543687));
#13624=CARTESIAN_POINT('Ctrl Pts',(-0.615966552324775,-0.224161999508995,
0.763642258217233));
#13625=CARTESIAN_POINT('Ctrl Pts',(-0.587792702767295,-0.203463743702801,
0.78555112003688));
#13626=CARTESIAN_POINT('Ctrl Pts',(-0.573915184558107,-0.190326085855194,
0.795684265985088));
#13627=CARTESIAN_POINT('Ctrl Pts',(-0.548874290046456,-0.159766064500479,
0.813159949759));
#13628=CARTESIAN_POINT('Ctrl Pts',(-0.537715343527944,-0.142345102874864,
0.820511285096538));
#13629=CARTESIAN_POINT('Ctrl Pts',(-0.517157748491652,-0.0999305678883309,
0.833661031856294));
#13630=CARTESIAN_POINT('Ctrl Pts',(-0.508899795931835,-0.0740444353928835,
0.838633903678357));
#13631=CARTESIAN_POINT('Ctrl Pts',(-0.504455939115716,-0.04763,0.841298510752801));
#13632=CARTESIAN_POINT('Origin',(-0.707106781186548,-0.04763,0.707106781186547));
#13633=CARTESIAN_POINT('Origin',(0.,-0.04763,0.));
#13634=CARTESIAN_POINT('',(-0.951592097314,-0.04763,0.238183666596899));
#13635=CARTESIAN_POINT('Origin',(0.,-0.04763,0.));
#13636=CARTESIAN_POINT('Origin',(-1.,-0.04763,-1.11022302462516E-16));
#13637=CARTESIAN_POINT('Origin',(-1.,0.,-1.11022302462516E-16));
#13638=CARTESIAN_POINT('',(-0.951592097314,-0.04763,-0.2381836665969));
#13639=CARTESIAN_POINT('',(-0.980948,-0.246942143572133,1.08514323328844E-18));
#13640=CARTESIAN_POINT('Ctrl Pts',(-0.951592097314,-0.04763,-0.238183666596899));
#13641=CARTESIAN_POINT('Ctrl Pts',(-0.952850216871763,-0.0740444353928835,
-0.233157223576062));
#13642=CARTESIAN_POINT('Ctrl Pts',(-0.955173119738174,-0.0999305678883309,
-0.223801617934946));
#13643=CARTESIAN_POINT('Ctrl Pts',(-0.960411259488514,-0.142345102874864,
-0.199966927975188));
#13644=CARTESIAN_POINT('Ctrl Pts',(-0.963103647174702,-0.159766064500479,
-0.1868781821531));
#13645=CARTESIAN_POINT('Ctrl Pts',(-0.968453058988463,-0.190326085855194,
-0.15681442133453));
#13646=CARTESIAN_POINT('Ctrl Pts',(-0.971100730005489,-0.203463743702801,
-0.139836317888043));
#13647=CARTESIAN_POINT('Ctrl Pts',(-0.975530745318961,-0.224161999508995,
-0.104422493053067));
#13648=CARTESIAN_POINT('Ctrl Pts',(-0.977553872336861,-0.232861760990032,
-0.0842175114474175));
#13649=CARTESIAN_POINT('Ctrl Pts',(-0.980270995488453,-0.244251601209411,
-0.0421062857595699));
#13650=CARTESIAN_POINT('Ctrl Pts',(-0.980948,-0.246942143572133,-0.0201990724523195));
#13651=CARTESIAN_POINT('Ctrl Pts',(-0.980948,-0.246942143572133,-1.17961196366423E-16));
#13652=CARTESIAN_POINT('Origin',(-1.,-0.04763,-1.11022302462516E-16));
#13653=CARTESIAN_POINT('Ctrl Pts',(-0.980948,-0.246942143572133,-1.17961196366423E-16));
#13654=CARTESIAN_POINT('Ctrl Pts',(-0.980948,-0.246942143572133,0.0201990724523192));
#13655=CARTESIAN_POINT('Ctrl Pts',(-0.980270995488453,-0.244251601209411,
0.0421062857595695));
#13656=CARTESIAN_POINT('Ctrl Pts',(-0.977553872336861,-0.232861760990032,
0.0842175114474169));
#13657=CARTESIAN_POINT('Ctrl Pts',(-0.975530745318961,-0.224161999508995,
0.104422493053066));
#13658=CARTESIAN_POINT('Ctrl Pts',(-0.971100730005489,-0.203463743702801,
0.139836317888042));
#13659=CARTESIAN_POINT('Ctrl Pts',(-0.968453058988463,-0.190326085855194,
0.15681442133453));
#13660=CARTESIAN_POINT('Ctrl Pts',(-0.963103647174702,-0.15976606450048,
0.1868781821531));
#13661=CARTESIAN_POINT('Ctrl Pts',(-0.960411259488514,-0.142345102874864,
0.199966927975188));
#13662=CARTESIAN_POINT('Ctrl Pts',(-0.955173119738174,-0.099930567888331,
0.223801617934945));
#13663=CARTESIAN_POINT('Ctrl Pts',(-0.952850216871763,-0.0740444353928835,
0.233157223576061));
#13664=CARTESIAN_POINT('Ctrl Pts',(-0.951592097314,-0.04763,0.238183666596899));
#13665=CARTESIAN_POINT('Origin',(0.,-0.04763,0.));
#13666=CARTESIAN_POINT('',(-0.841298510752802,-0.04763,-0.504455939115715));
#13667=CARTESIAN_POINT('Origin',(0.,-0.04763,0.));
#13668=CARTESIAN_POINT('Origin',(-0.707106781186547,-0.04763,-0.707106781186548));
#13669=CARTESIAN_POINT('Origin',(-0.707106781186547,0.,-0.707106781186548));
#13670=CARTESIAN_POINT('',(-0.504455939115715,-0.04763,-0.841298510752802));
#13671=CARTESIAN_POINT('Ctrl Pts',(-0.504455939115715,-0.04763,-0.841298510752802));
#13672=CARTESIAN_POINT('Ctrl Pts',(-0.508899795931835,-0.0740444353928835,
-0.838633903678357));
#13673=CARTESIAN_POINT('Ctrl Pts',(-0.517157748491652,-0.0999305678883309,
-0.833661031856294));
#13674=CARTESIAN_POINT('Ctrl Pts',(-0.537715343527944,-0.142345102874864,
-0.820511285096538));
#13675=CARTESIAN_POINT('Ctrl Pts',(-0.548874290046456,-0.159766064500479,
-0.813159949759));
#13676=CARTESIAN_POINT('Ctrl Pts',(-0.573915184558107,-0.190326085855194,
-0.795684265985089));
#13677=CARTESIAN_POINT('Ctrl Pts',(-0.587792702767295,-0.203463743702801,
-0.78555112003688));
#13678=CARTESIAN_POINT('Ctrl Pts',(-0.615966552324775,-0.224161999508995,
-0.763642258217233));
#13679=CARTESIAN_POINT('Ctrl Pts',(-0.631684198665438,-0.232861760990032,
-0.750785745543687));
#13680=CARTESIAN_POINT('Ctrl Pts',(-0.663382628119203,-0.244251601209411,
-0.722929908501543));
#13681=CARTESIAN_POINT('Ctrl Pts',(-0.679352081686668,-0.246942143572133,
-0.707917883896095));
#13682=CARTESIAN_POINT('Ctrl Pts',(-0.707917883896095,-0.246942143572133,
-0.679352081686668));
#13683=CARTESIAN_POINT('Ctrl Pts',(-0.722929908501543,-0.244251601209411,
-0.663382628119203));
#13684=CARTESIAN_POINT('Ctrl Pts',(-0.750785745543687,-0.232861760990032,
-0.631684198665439));
#13685=CARTESIAN_POINT('Ctrl Pts',(-0.763642258217232,-0.224161999508995,
-0.615966552324775));
#13686=CARTESIAN_POINT('Ctrl Pts',(-0.78555112003688,-0.203463743702801,
-0.587792702767295));
#13687=CARTESIAN_POINT('Ctrl Pts',(-0.795684265985088,-0.190326085855194,
-0.573915184558107));
#13688=CARTESIAN_POINT('Ctrl Pts',(-0.813159949759,-0.15976606450048,-0.548874290046456));
#13689=CARTESIAN_POINT('Ctrl Pts',(-0.820511285096538,-0.142345102874864,
-0.537715343527944));
#13690=CARTESIAN_POINT('Ctrl Pts',(-0.833661031856294,-0.0999305678883311,
-0.517157748491652));
#13691=CARTESIAN_POINT('Ctrl Pts',(-0.838633903678357,-0.0740444353928836,
-0.508899795931835));
#13692=CARTESIAN_POINT('Ctrl Pts',(-0.841298510752801,-0.04763,-0.504455939115715));
#13693=CARTESIAN_POINT('Origin',(-0.707106781186547,-0.04763,-0.707106781186548));
#13694=CARTESIAN_POINT('Origin',(0.,-0.04763,0.));
#13695=CARTESIAN_POINT('',(-0.238183666596899,-0.04763,-0.951592097314));
#13696=CARTESIAN_POINT('Origin',(0.,-0.04763,0.));
#13697=CARTESIAN_POINT('Origin',(5.55111512312578E-17,-0.04763,-1.));
#13698=CARTESIAN_POINT('Origin',(5.55111512312578E-17,0.,-1.));
#13699=CARTESIAN_POINT('',(0.238183666596899,-0.04763,-0.951592097314));
#13700=CARTESIAN_POINT('Ctrl Pts',(0.238183666596899,-0.04763,-0.951592097314));
#13701=CARTESIAN_POINT('Ctrl Pts',(0.233157223576062,-0.0740444353928835,
-0.952850216871763));
#13702=CARTESIAN_POINT('Ctrl Pts',(0.223801617934946,-0.099930567888331,
-0.955173119738174));
#13703=CARTESIAN_POINT('Ctrl Pts',(0.199966927975188,-0.142345102874864,
-0.960411259488514));
#13704=CARTESIAN_POINT('Ctrl Pts',(0.1868781821531,-0.15976606450048,-0.963103647174702));
#13705=CARTESIAN_POINT('Ctrl Pts',(0.15681442133453,-0.190326085855194,
-0.968453058988463));
#13706=CARTESIAN_POINT('Ctrl Pts',(0.139836317888042,-0.203463743702801,
-0.971100730005489));
#13707=CARTESIAN_POINT('Ctrl Pts',(0.104422493053067,-0.224161999508995,
-0.975530745318961));
#13708=CARTESIAN_POINT('Ctrl Pts',(0.0842175114474173,-0.232861760990032,
-0.977553872336861));
#13709=CARTESIAN_POINT('Ctrl Pts',(0.0421062857595698,-0.244251601209411,
-0.980270995488453));
#13710=CARTESIAN_POINT('Ctrl Pts',(0.0201990724523194,-0.246942143572133,
-0.980948));
#13711=CARTESIAN_POINT('Ctrl Pts',(-0.0201990724523193,-0.246942143572133,
-0.980948));
#13712=CARTESIAN_POINT('Ctrl Pts',(-0.0421062857595697,-0.244251601209411,
-0.980270995488453));
#13713=CARTESIAN_POINT('Ctrl Pts',(-0.0842175114474171,-0.232861760990032,
-0.977553872336861));
#13714=CARTESIAN_POINT('Ctrl Pts',(-0.104422493053067,-0.224161999508995,
-0.975530745318961));
#13715=CARTESIAN_POINT('Ctrl Pts',(-0.139836317888042,-0.203463743702801,
-0.971100730005489));
#13716=CARTESIAN_POINT('Ctrl Pts',(-0.15681442133453,-0.190326085855194,
-0.968453058988463));
#13717=CARTESIAN_POINT('Ctrl Pts',(-0.1868781821531,-0.15976606450048,-0.963103647174702));
#13718=CARTESIAN_POINT('Ctrl Pts',(-0.199966927975188,-0.142345102874864,
-0.960411259488514));
#13719=CARTESIAN_POINT('Ctrl Pts',(-0.223801617934945,-0.099930567888331,
-0.955173119738174));
#13720=CARTESIAN_POINT('Ctrl Pts',(-0.233157223576062,-0.0740444353928835,
-0.952850216871763));
#13721=CARTESIAN_POINT('Ctrl Pts',(-0.238183666596899,-0.0476299999999999,
-0.951592097314));
#13722=CARTESIAN_POINT('Origin',(5.55111512312578E-17,-0.04763,-1.));
#13723=CARTESIAN_POINT('Origin',(0.,-0.04763,0.));
#13724=CARTESIAN_POINT('',(0.504455939115715,-0.04763,-0.841298510752802));
#13725=CARTESIAN_POINT('Origin',(0.,-0.04763,0.));
#13726=CARTESIAN_POINT('Origin',(0.707106781186548,-0.04763,-0.707106781186547));
#13727=CARTESIAN_POINT('Origin',(0.707106781186548,0.,-0.707106781186547));
#13728=CARTESIAN_POINT('',(0.841298510752802,-0.04763,-0.504455939115715));
#13729=CARTESIAN_POINT('Ctrl Pts',(0.841298510752802,-0.04763,-0.504455939115715));
#13730=CARTESIAN_POINT('Ctrl Pts',(0.838633903678357,-0.0740444353928835,
-0.508899795931835));
#13731=CARTESIAN_POINT('Ctrl Pts',(0.833661031856294,-0.0999305678883309,
-0.517157748491652));
#13732=CARTESIAN_POINT('Ctrl Pts',(0.820511285096538,-0.142345102874864,
-0.537715343527944));
#13733=CARTESIAN_POINT('Ctrl Pts',(0.813159949759,-0.159766064500479,-0.548874290046456));
#13734=CARTESIAN_POINT('Ctrl Pts',(0.795684265985088,-0.190326085855194,
-0.573915184558107));
#13735=CARTESIAN_POINT('Ctrl Pts',(0.78555112003688,-0.203463743702801,
-0.587792702767295));
#13736=CARTESIAN_POINT('Ctrl Pts',(0.763642258217233,-0.224161999508995,
-0.615966552324775));
#13737=CARTESIAN_POINT('Ctrl Pts',(0.750785745543687,-0.232861760990032,
-0.631684198665438));
#13738=CARTESIAN_POINT('Ctrl Pts',(0.722929908501543,-0.244251601209411,
-0.663382628119203));
#13739=CARTESIAN_POINT('Ctrl Pts',(0.707917883896095,-0.246942143572133,
-0.679352081686668));
#13740=CARTESIAN_POINT('Ctrl Pts',(0.679352081686668,-0.246942143572133,
-0.707917883896095));
#13741=CARTESIAN_POINT('Ctrl Pts',(0.663382628119203,-0.244251601209411,
-0.722929908501543));
#13742=CARTESIAN_POINT('Ctrl Pts',(0.631684198665438,-0.232861760990032,
-0.750785745543687));
#13743=CARTESIAN_POINT('Ctrl Pts',(0.615966552324775,-0.224161999508995,
-0.763642258217232));
#13744=CARTESIAN_POINT('Ctrl Pts',(0.587792702767295,-0.203463743702801,
-0.78555112003688));
#13745=CARTESIAN_POINT('Ctrl Pts',(0.573915184558107,-0.190326085855194,
-0.795684265985088));
#13746=CARTESIAN_POINT('Ctrl Pts',(0.548874290046456,-0.159766064500479,
-0.813159949759));
#13747=CARTESIAN_POINT('Ctrl Pts',(0.537715343527944,-0.142345102874864,
-0.820511285096538));
#13748=CARTESIAN_POINT('Ctrl Pts',(0.517157748491652,-0.099930567888331,
-0.833661031856294));
#13749=CARTESIAN_POINT('Ctrl Pts',(0.508899795931835,-0.0740444353928835,
-0.838633903678357));
#13750=CARTESIAN_POINT('Ctrl Pts',(0.504455939115715,-0.04763,-0.841298510752801));
#13751=CARTESIAN_POINT('Origin',(0.707106781186548,-0.04763,-0.707106781186547));
#13752=CARTESIAN_POINT('Origin',(0.,-0.166705,0.));
#13753=CARTESIAN_POINT('',(-0.980948,-0.28578,1.20131482833E-16));
#13754=CARTESIAN_POINT('Origin',(0.,-0.28578,0.));
#13755=CARTESIAN_POINT('',(-0.980948,-0.166705,1.20131482833E-16));
#13756=CARTESIAN_POINT('',(0.951592097314,-0.04763,0.238183666596899));
#13757=CARTESIAN_POINT('Origin',(0.,-0.04763,0.));
#13758=CARTESIAN_POINT('',(0.951592097314,-0.04763,-0.238183666596899));
#13759=CARTESIAN_POINT('Ctrl Pts',(0.951592097314,-0.04763,0.238183666596899));
#13760=CARTESIAN_POINT('Ctrl Pts',(0.952850216871763,-0.0740444353928835,
0.233157223576062));
#13761=CARTESIAN_POINT('Ctrl Pts',(0.955173119738174,-0.099930567888331,
0.223801617934945));
#13762=CARTESIAN_POINT('Ctrl Pts',(0.960411259488514,-0.142345102874864,
0.199966927975188));
#13763=CARTESIAN_POINT('Ctrl Pts',(0.963103647174702,-0.15976606450048,
0.1868781821531));
#13764=CARTESIAN_POINT('Ctrl Pts',(0.968453058988463,-0.190326085855194,
0.15681442133453));
#13765=CARTESIAN_POINT('Ctrl Pts',(0.971100730005489,-0.203463743702801,
0.139836317888042));
#13766=CARTESIAN_POINT('Ctrl Pts',(0.975530745318961,-0.224161999508995,
0.104422493053067));
#13767=CARTESIAN_POINT('Ctrl Pts',(0.977553872336861,-0.232861760990032,
0.0842175114474172));
#13768=CARTESIAN_POINT('Ctrl Pts',(0.980270995488453,-0.244251601209411,
0.0421062857595697));
#13769=CARTESIAN_POINT('Ctrl Pts',(0.980948,-0.246942143572133,0.0201990724523194));
#13770=CARTESIAN_POINT('Ctrl Pts',(0.980948,-0.246942143572133,-0.0201990724523194));
#13771=CARTESIAN_POINT('Ctrl Pts',(0.980270995488453,-0.244251601209411,
-0.0421062857595697));
#13772=CARTESIAN_POINT('Ctrl Pts',(0.977553872336861,-0.232861760990032,
-0.0842175114474172));
#13773=CARTESIAN_POINT('Ctrl Pts',(0.975530745318961,-0.224161999508995,
-0.104422493053067));
#13774=CARTESIAN_POINT('Ctrl Pts',(0.971100730005489,-0.203463743702801,
-0.139836317888042));
#13775=CARTESIAN_POINT('Ctrl Pts',(0.968453058988463,-0.190326085855194,
-0.15681442133453));
#13776=CARTESIAN_POINT('Ctrl Pts',(0.963103647174702,-0.15976606450048,
-0.1868781821531));
#13777=CARTESIAN_POINT('Ctrl Pts',(0.960411259488514,-0.142345102874864,
-0.199966927975188));
#13778=CARTESIAN_POINT('Ctrl Pts',(0.955173119738174,-0.099930567888331,
-0.223801617934945));
#13779=CARTESIAN_POINT('Ctrl Pts',(0.952850216871763,-0.0740444353928835,
-0.233157223576062));
#13780=CARTESIAN_POINT('Ctrl Pts',(0.951592097314,-0.0476299999999999,-0.238183666596899));
#13781=CARTESIAN_POINT('Origin',(0.,-0.04763,0.));
#13782=CARTESIAN_POINT('Origin',(0.,-0.04763,0.));
#13783=CARTESIAN_POINT('Origin',(1.,-0.04763,0.));
#13784=CARTESIAN_POINT('Origin',(1.,0.,0.));
#13785=CARTESIAN_POINT('Origin',(1.,-0.04763,0.));
#13786=CARTESIAN_POINT('Origin',(0.,-0.28578,0.));
#13787=CARTESIAN_POINT('Origin',(0.,-0.04763,0.));
#13788=CARTESIAN_POINT('',(0.,0.,0.));
#13789=CARTESIAN_POINT('Origin',(1.013815,0.445,0.));
#13790=CARTESIAN_POINT('',(-1.013815,0.445,-1.24156529467757E-16));
#13791=CARTESIAN_POINT('Origin',(0.,0.445,0.));
#13792=CARTESIAN_POINT('',(-0.991185,0.445,-1.21385153761287E-16));
#13793=CARTESIAN_POINT('Origin',(0.,0.445,0.));
#13794=CARTESIAN_POINT('Origin',(0.,0.4075,0.));
#13795=CARTESIAN_POINT('',(-1.013815,0.37,-1.24156529467757E-16));
#13796=CARTESIAN_POINT('Origin',(0.,0.37,0.));
#13797=CARTESIAN_POINT('',(-1.013815,0.4075,-1.24156529467757E-16));
#13798=CARTESIAN_POINT('Origin',(0.991185,0.37,0.));
#13799=CARTESIAN_POINT('',(-0.991185,0.37,-1.21385153761287E-16));
#13800=CARTESIAN_POINT('Origin',(0.,0.37,0.));
#13801=CARTESIAN_POINT('Origin',(0.,0.4075,0.));
#13802=CARTESIAN_POINT('',(-0.991185,0.4075,-1.21385153761287E-16));
#13803=CARTESIAN_POINT('Origin',(1.013815,-0.37,0.));
#13804=CARTESIAN_POINT('',(-1.013815,-0.37,-1.24156529467757E-16));
#13805=CARTESIAN_POINT('Origin',(0.,-0.37,0.));
#13806=CARTESIAN_POINT('',(-0.991185,-0.37,-1.21385153761287E-16));
#13807=CARTESIAN_POINT('Origin',(0.,-0.37,0.));
#13808=CARTESIAN_POINT('Origin',(0.,-0.4075,0.));
#13809=CARTESIAN_POINT('',(-1.013815,-0.445,-1.24156529467757E-16));
#13810=CARTESIAN_POINT('Origin',(0.,-0.445,0.));
#13811=CARTESIAN_POINT('',(-1.013815,-0.4075,-1.24156529467757E-16));
#13812=CARTESIAN_POINT('Origin',(0.991185,-0.445,0.));
#13813=CARTESIAN_POINT('',(-0.991185,-0.445,-1.21385153761287E-16));
#13814=CARTESIAN_POINT('Origin',(0.,-0.445,0.));
#13815=CARTESIAN_POINT('Origin',(0.,-0.4075,0.));
#13816=CARTESIAN_POINT('',(-0.991185,-0.4075,-1.21385153761287E-16));
#13817=CARTESIAN_POINT('',(0.,0.,0.));
#13818=CARTESIAN_POINT('',(0.,0.,0.));
#13819=CARTESIAN_POINT('',(0.,0.,0.));
#13820=CARTESIAN_POINT('',(0.,0.,0.));
#13821=CARTESIAN_POINT('',(0.,0.,0.));
#13822=CARTESIAN_POINT('',(0.,0.,0.));
#13823=CARTESIAN_POINT('Origin',(0.0866025403784439,-0.4,-0.15));
#13824=CARTESIAN_POINT('',(0.173205080756888,-0.4,0.));
#13825=CARTESIAN_POINT('',(0.0866025403784439,-0.4,-0.15));
#13826=CARTESIAN_POINT('',(0.173205080756888,-0.4,0.));
#13827=CARTESIAN_POINT('',(0.0866025403784439,-0.64,-0.15));
#13828=CARTESIAN_POINT('',(0.0866025403784439,-0.4,-0.15));
#13829=CARTESIAN_POINT('',(0.173205080756888,-0.64,0.));
#13830=CARTESIAN_POINT('',(0.173205080756888,-0.64,0.));
#13831=CARTESIAN_POINT('',(0.173205080756888,-0.4,0.));
#13832=CARTESIAN_POINT('Origin',(-0.0866025403784438,-0.4,-0.15));
#13833=CARTESIAN_POINT('',(-0.0866025403784438,-0.4,-0.15));
#13834=CARTESIAN_POINT('',(0.0866025403784439,-0.4,-0.15));
#13835=CARTESIAN_POINT('',(-0.0866025403784438,-0.64,-0.15));
#13836=CARTESIAN_POINT('',(-0.0866025403784438,-0.4,-0.15));
#13837=CARTESIAN_POINT('',(0.0866025403784439,-0.64,-0.15));
#13838=CARTESIAN_POINT('Origin',(-0.173205080756888,-0.4,-2.77555756156289E-17));
#13839=CARTESIAN_POINT('',(-0.173205080756888,-0.4,-2.12115047744981E-17));
#13840=CARTESIAN_POINT('',(-0.0866025403784438,-0.4,-0.15));
#13841=CARTESIAN_POINT('',(-0.173205080756888,-0.64,-2.77555756156289E-17));
#13842=CARTESIAN_POINT('',(-0.173205080756888,-0.4,-2.12115047744981E-17));
#13843=CARTESIAN_POINT('',(-0.0866025403784438,-0.64,-0.15));
#13844=CARTESIAN_POINT('Origin',(-0.0866025403784439,-0.4,0.15));
#13845=CARTESIAN_POINT('',(-0.0866025403784439,-0.4,0.15));
#13846=CARTESIAN_POINT('',(-0.173205080756888,-0.4,-2.12115047744981E-17));
#13847=CARTESIAN_POINT('',(-0.0866025403784439,-0.64,0.15));
#13848=CARTESIAN_POINT('',(-0.0866025403784439,-0.4,0.15));
#13849=CARTESIAN_POINT('',(-0.173205080756888,-0.64,-2.12115047744981E-17));
#13850=CARTESIAN_POINT('Origin',(0.0866025403784439,-0.4,0.15));
#13851=CARTESIAN_POINT('',(0.0866025403784439,-0.4,0.15));
#13852=CARTESIAN_POINT('',(-0.0866025403784439,-0.4,0.15));
#13853=CARTESIAN_POINT('',(0.0866025403784439,-0.64,0.15));
#13854=CARTESIAN_POINT('',(0.0866025403784439,-0.4,0.15));
#13855=CARTESIAN_POINT('',(-0.0866025403784439,-0.64,0.15));
#13856=CARTESIAN_POINT('Origin',(0.173205080756888,-0.4,0.));
#13857=CARTESIAN_POINT('',(0.0866025403784439,-0.4,0.15));
#13858=CARTESIAN_POINT('',(0.0866025403784439,-0.64,0.15));
#13859=CARTESIAN_POINT('Origin',(0.,-0.4,-2.77555756156289E-17));
#13860=CARTESIAN_POINT('Origin',(0.,-0.64,-2.77555756156289E-17));
#13861=CARTESIAN_POINT('Origin',(0.,-1.,0.));
#13862=CARTESIAN_POINT('',(-0.1954,-1.,2.39295984553393E-17));
#13863=CARTESIAN_POINT('Origin',(0.,-1.,0.));
#13864=CARTESIAN_POINT('Origin',(0.3,0.4,0.));
#13865=CARTESIAN_POINT('',(-0.3,0.4,-3.67394039744206E-17));
#13866=CARTESIAN_POINT('Origin',(0.,0.4,0.));
#13867=CARTESIAN_POINT('Origin',(0.,0.375,0.));
#13868=CARTESIAN_POINT('',(-0.35,0.35,-4.28626379701573E-17));
#13869=CARTESIAN_POINT('Origin',(0.,0.35,0.));
#13870=CARTESIAN_POINT('',(-0.325,0.375,-3.9801020972289E-17));
#13871=CARTESIAN_POINT('Origin',(0.,0.19,0.));
#13872=CARTESIAN_POINT('',(-0.35,0.03,-4.28626379701574E-17));
#13873=CARTESIAN_POINT('Origin',(0.,0.03,0.));
#13874=CARTESIAN_POINT('',(-0.35,0.19,-4.28626379701574E-17));
#13875=CARTESIAN_POINT('Origin',(0.,0.0149999999999999,0.));
#13876=CARTESIAN_POINT('',(-0.32,-3.29597460435593E-17,-3.91886975727153E-17));
#13877=CARTESIAN_POINT('Origin',(0.,0.,0.));
#13878=CARTESIAN_POINT('',(-0.335,0.0149999999999999,-4.10256677714363E-17));
#13879=CARTESIAN_POINT('Origin',(0.22,0.,0.));
#13880=CARTESIAN_POINT('',(-0.22,-6.93889390390723E-18,-2.69422295812418E-17));
#13881=CARTESIAN_POINT('Origin',(0.,0.,0.));
#13882=CARTESIAN_POINT('Origin',(0.,-0.02,0.));
#13883=CARTESIAN_POINT('',(-0.1954,-0.0492,2.39295984553393E-17));
#13884=CARTESIAN_POINT('Origin',(0.,-0.0492,0.));
#13885=CARTESIAN_POINT('',(-0.21,-0.02,-2.57175827820944E-17));
#13886=CARTESIAN_POINT('Origin',(0.,-0.8,0.));
#13887=CARTESIAN_POINT('',(-0.1954,-0.8,-2.39295984553393E-17));
#13888=CARTESIAN_POINT('',(0.,0.,0.));
#13889=CARTESIAN_POINT('',(0.,0.,0.));
#13890=CARTESIAN_POINT('',(0.,0.,0.));
#13891=CARTESIAN_POINT('',(0.,0.,0.));
#13892=CARTESIAN_POINT('',(0.,0.,0.));
#13893=CARTESIAN_POINT('',(0.,0.,0.));
#13894=CARTESIAN_POINT('',(0.,0.,0.));
#13895=CARTESIAN_POINT('',(0.,0.,0.));
#13896=CARTESIAN_POINT('',(0.,-0.6,8.));
#13897=CARTESIAN_POINT('',(0.,0.6,8.));
#13898=CARTESIAN_POINT('',(1.23743686707646,-1.4,9.23743686707646));
#13899=CARTESIAN_POINT('',(-1.23743686707646,-1.4,9.23743686707646));
#13900=CARTESIAN_POINT('',(-1.23743686707646,-1.4,6.76256313292354));
#13901=CARTESIAN_POINT('',(1.23743686707646,-1.4,6.76256313292354));
#13902=CARTESIAN_POINT('',(1.23743686707646,1.4,9.23743686707646));
#13903=CARTESIAN_POINT('',(-1.23743686707646,1.4,9.23743686707646));
#13904=CARTESIAN_POINT('',(-1.23743686707646,1.4,6.76256313292354));
#13905=CARTESIAN_POINT('',(1.23743686707646,1.4,6.76256313292354));
#13906=CARTESIAN_POINT('',(20.,-0.6,8.));
#13907=CARTESIAN_POINT('',(20.,0.6,8.));
#13908=CARTESIAN_POINT('',(21.2374368670765,-1.4,9.23743686707646));
#13909=CARTESIAN_POINT('',(18.7625631329235,-1.4,9.23743686707646));
#13910=CARTESIAN_POINT('',(18.7625631329235,-1.4,6.76256313292354));
#13911=CARTESIAN_POINT('',(21.2374368670765,-1.4,6.76256313292354));
#13912=CARTESIAN_POINT('',(21.2374368670765,1.4,9.23743686707646));
#13913=CARTESIAN_POINT('',(18.7625631329235,1.4,9.23743686707646));
#13914=CARTESIAN_POINT('',(18.7625631329235,1.4,6.76256313292354));
#13915=CARTESIAN_POINT('',(21.2374368670765,1.4,6.76256313292354));
#13916=CARTESIAN_POINT('',(0.,0.,0.));
#13917=CARTESIAN_POINT('',(0.,0.,0.));
#13918=CARTESIAN_POINT('',(0.,0.,0.));
#13919=CARTESIAN_POINT('',(0.,0.,0.));
#13920=CARTESIAN_POINT('',(0.,0.,0.));
#13921=CARTESIAN_POINT('',(0.,0.,0.));
#13922=CARTESIAN_POINT('',(0.,0.,0.));
#13923=CARTESIAN_POINT('',(0.,-0.6,14.));
#13924=CARTESIAN_POINT('',(0.,0.6,14.));
#13925=CARTESIAN_POINT('',(1.23743686707646,-1.4,15.2374368670765));
#13926=CARTESIAN_POINT('',(-1.23743686707646,-1.4,15.2374368670765));
#13927=CARTESIAN_POINT('',(-1.23743686707646,-1.4,12.7625631329235));
#13928=CARTESIAN_POINT('',(1.23743686707646,-1.4,12.7625631329235));
#13929=CARTESIAN_POINT('',(1.23743686707646,1.4,15.2374368670765));
#13930=CARTESIAN_POINT('',(-1.23743686707646,1.4,15.2374368670765));
#13931=CARTESIAN_POINT('',(-1.23743686707646,1.4,12.7625631329235));
#13932=CARTESIAN_POINT('',(1.23743686707646,1.4,12.7625631329235));
#13933=CARTESIAN_POINT('',(20.,-0.6,14.));
#13934=CARTESIAN_POINT('',(20.,0.6,14.));
#13935=CARTESIAN_POINT('',(21.2374368670765,-1.4,15.2374368670765));
#13936=CARTESIAN_POINT('',(18.7625631329235,-1.4,15.2374368670765));
#13937=CARTESIAN_POINT('',(18.7625631329235,-1.4,12.7625631329235));
#13938=CARTESIAN_POINT('',(21.2374368670765,-1.4,12.7625631329235));
#13939=CARTESIAN_POINT('',(21.2374368670765,1.4,15.2374368670765));
#13940=CARTESIAN_POINT('',(18.7625631329235,1.4,15.2374368670765));
#13941=CARTESIAN_POINT('',(18.7625631329235,1.4,12.7625631329235));
#13942=CARTESIAN_POINT('',(21.2374368670765,1.4,12.7625631329235));
#13943=CARTESIAN_POINT('',(0.,0.,0.));
#13944=CARTESIAN_POINT('',(0.,0.,0.));
#13945=CARTESIAN_POINT('Origin',(21.15,2.8,14.));
#13946=CARTESIAN_POINT('',(20.985,2.9,14.));
#13947=CARTESIAN_POINT('Origin',(21.15,2.9,14.));
#13948=CARTESIAN_POINT('',(20.985,3.9,14.));
#13949=CARTESIAN_POINT('',(20.985,2.8,14.));
#13950=CARTESIAN_POINT('Origin',(21.15,3.9,14.));
#13951=CARTESIAN_POINT('Origin',(19.425,2.8,14.9959292143521));
#13952=CARTESIAN_POINT('',(19.26,2.9,14.9959292143521));
#13953=CARTESIAN_POINT('Origin',(19.425,2.9,14.9959292143521));
#13954=CARTESIAN_POINT('',(19.26,3.9,14.9959292143521));
#13955=CARTESIAN_POINT('',(19.26,2.8,14.9959292143521));
#13956=CARTESIAN_POINT('Origin',(19.425,3.9,14.9959292143521));
#13957=CARTESIAN_POINT('Origin',(19.425,2.8,13.0040707856479));
#13958=CARTESIAN_POINT('',(19.26,2.9,13.0040707856479));
#13959=CARTESIAN_POINT('Origin',(19.425,2.9,13.0040707856479));
#13960=CARTESIAN_POINT('',(19.26,3.9,13.0040707856479));
#13961=CARTESIAN_POINT('',(19.26,2.8,13.0040707856479));
#13962=CARTESIAN_POINT('Origin',(19.425,3.9,13.0040707856479));
#13963=CARTESIAN_POINT('Origin',(20.,2.8,14.));
#13964=CARTESIAN_POINT('',(19.495,2.9,14.));
#13965=CARTESIAN_POINT('Origin',(20.,2.9,14.));
#13966=CARTESIAN_POINT('',(19.495,3.9,14.));
#13967=CARTESIAN_POINT('',(19.495,2.8,14.));
#13968=CARTESIAN_POINT('Origin',(20.,3.9,14.));
#13969=CARTESIAN_POINT('Origin',(21.15,2.8,8.));
#13970=CARTESIAN_POINT('',(20.985,2.9,8.));
#13971=CARTESIAN_POINT('Origin',(21.15,2.9,8.));
#13972=CARTESIAN_POINT('',(20.985,3.9,8.));
#13973=CARTESIAN_POINT('',(20.985,2.8,8.));
#13974=CARTESIAN_POINT('Origin',(21.15,3.9,8.));
#13975=CARTESIAN_POINT('Origin',(19.425,2.8,8.9959292143521));
#13976=CARTESIAN_POINT('',(19.26,2.9,8.9959292143521));
#13977=CARTESIAN_POINT('Origin',(19.425,2.9,8.9959292143521));
#13978=CARTESIAN_POINT('',(19.26,3.9,8.9959292143521));
#13979=CARTESIAN_POINT('',(19.26,2.8,8.9959292143521));
#13980=CARTESIAN_POINT('Origin',(19.425,3.9,8.9959292143521));
#13981=CARTESIAN_POINT('Origin',(19.425,2.8,7.0040707856479));
#13982=CARTESIAN_POINT('',(19.26,2.9,7.0040707856479));
#13983=CARTESIAN_POINT('Origin',(19.425,2.9,7.0040707856479));
#13984=CARTESIAN_POINT('',(19.26,3.9,7.0040707856479));
#13985=CARTESIAN_POINT('',(19.26,2.8,7.0040707856479));
#13986=CARTESIAN_POINT('Origin',(19.425,3.9,7.0040707856479));
#13987=CARTESIAN_POINT('Origin',(20.,2.8,8.));
#13988=CARTESIAN_POINT('',(19.495,2.9,8.));
#13989=CARTESIAN_POINT('Origin',(20.,2.9,8.));
#13990=CARTESIAN_POINT('',(19.495,3.9,8.));
#13991=CARTESIAN_POINT('',(19.495,2.8,8.));
#13992=CARTESIAN_POINT('Origin',(20.,3.9,8.));
#13993=CARTESIAN_POINT('Origin',(19.,8.,15.9));
#13994=CARTESIAN_POINT('',(18.67,8.,16.));
#13995=CARTESIAN_POINT('Origin',(19.,8.,16.));
#13996=CARTESIAN_POINT('',(18.67,8.,17.));
#13997=CARTESIAN_POINT('',(18.67,8.,15.9));
#13998=CARTESIAN_POINT('Origin',(19.,8.,17.));
#13999=CARTESIAN_POINT('Origin',(26.,4.5,15.9));
#14000=CARTESIAN_POINT('',(25.67,4.5,16.));
#14001=CARTESIAN_POINT('Origin',(26.,4.5,16.));
#14002=CARTESIAN_POINT('',(25.67,4.5,17.));
#14003=CARTESIAN_POINT('',(25.67,4.5,15.9));
#14004=CARTESIAN_POINT('Origin',(26.,4.5,17.));
#14005=CARTESIAN_POINT('Origin',(19.,4.5,15.9));
#14006=CARTESIAN_POINT('',(18.67,4.5,16.));
#14007=CARTESIAN_POINT('Origin',(19.,4.5,16.));
#14008=CARTESIAN_POINT('',(18.67,4.5,17.));
#14009=CARTESIAN_POINT('',(18.67,4.5,15.9));
#14010=CARTESIAN_POINT('Origin',(19.,4.5,17.));
#14011=CARTESIAN_POINT('Origin',(26.,8.,15.9));
#14012=CARTESIAN_POINT('',(25.67,8.,16.));
#14013=CARTESIAN_POINT('Origin',(26.,8.,16.));
#14014=CARTESIAN_POINT('',(25.67,8.,17.));
#14015=CARTESIAN_POINT('',(25.67,8.,15.9));
#14016=CARTESIAN_POINT('Origin',(26.,8.,17.));
#14017=CARTESIAN_POINT('Origin',(27.5,9.9,16.));
#14018=CARTESIAN_POINT('',(27.5,9.9,16.));
#14019=CARTESIAN_POINT('',(17.5,9.9,16.));
#14020=CARTESIAN_POINT('',(27.5,9.9,16.));
#14021=CARTESIAN_POINT('',(17.5,9.9,17.));
#14022=CARTESIAN_POINT('',(17.5,9.9,16.));
#14023=CARTESIAN_POINT('',(27.5,9.9,17.));
#14024=CARTESIAN_POINT('',(27.5,9.9,17.));
#14025=CARTESIAN_POINT('',(27.5,9.9,16.));
#14026=CARTESIAN_POINT('Origin',(27.5,2.9,16.));
#14027=CARTESIAN_POINT('',(27.5,2.9,16.));
#14028=CARTESIAN_POINT('',(27.5,2.9,16.));
#14029=CARTESIAN_POINT('',(27.5,2.9,17.));
#14030=CARTESIAN_POINT('',(27.5,2.9,17.));
#14031=CARTESIAN_POINT('',(27.5,2.9,16.));
#14032=CARTESIAN_POINT('Origin',(22.5,6.4,17.));
#14033=CARTESIAN_POINT('',(17.5,2.9,17.));
#14034=CARTESIAN_POINT('',(17.5,9.9,17.));
#14035=CARTESIAN_POINT('',(17.5,2.9,17.));
#14036=CARTESIAN_POINT('Origin',(22.5,6.4,16.));
#14037=CARTESIAN_POINT('',(22.5,3.9,16.));
#14038=CARTESIAN_POINT('',(17.5,3.9,16.));
#14039=CARTESIAN_POINT('',(22.5,3.9,16.));
#14040=CARTESIAN_POINT('',(17.5,9.9,16.));
#14041=CARTESIAN_POINT('',(22.5,2.9,16.));
#14042=CARTESIAN_POINT('',(17.5,2.9,16.));
#14043=CARTESIAN_POINT('',(22.5,2.9,16.));
#14044=CARTESIAN_POINT('Origin',(22.5,3.9,6.));
#14045=CARTESIAN_POINT('',(22.5,3.9,6.));
#14046=CARTESIAN_POINT('',(17.5,3.9,6.));
#14047=CARTESIAN_POINT('',(22.5,3.9,6.));
#14048=CARTESIAN_POINT('',(17.5,3.9,6.));
#14049=CARTESIAN_POINT('',(22.5,3.9,6.));
#14050=CARTESIAN_POINT('Origin',(22.5,2.9,6.));
#14051=CARTESIAN_POINT('',(22.5,2.9,6.));
#14052=CARTESIAN_POINT('',(22.5,2.9,6.));
#14053=CARTESIAN_POINT('',(22.5,2.9,6.));
#14054=CARTESIAN_POINT('Origin',(17.5,2.9,6.));
#14055=CARTESIAN_POINT('',(17.5,2.9,6.));
#14056=CARTESIAN_POINT('',(17.5,2.9,6.));
#14057=CARTESIAN_POINT('',(17.5,2.9,6.));
#14058=CARTESIAN_POINT('Origin',(17.5,3.9,6.));
#14059=CARTESIAN_POINT('',(17.5,3.9,6.));
#14060=CARTESIAN_POINT('Origin',(20.,3.4,6.));
#14061=CARTESIAN_POINT('',(0.,0.,0.));
#14062=CARTESIAN_POINT('Origin',(20.,-1.7,8.));
#14063=CARTESIAN_POINT('',(19.835,-1.6,8.));
#14064=CARTESIAN_POINT('Origin',(20.,-1.6,8.));
#14065=CARTESIAN_POINT('',(19.835,0.,8.));
#14066=CARTESIAN_POINT('',(19.835,-1.7,8.));
#14067=CARTESIAN_POINT('Origin',(20.,0.,8.));
#14068=CARTESIAN_POINT('Origin',(20.,0.,8.));
#14069=CARTESIAN_POINT('Origin',(21.15,2.4,8.));
#14070=CARTESIAN_POINT('',(20.925,2.5,8.));
#14071=CARTESIAN_POINT('Origin',(21.15,2.5,8.));
#14072=CARTESIAN_POINT('',(20.925,2.9,8.));
#14073=CARTESIAN_POINT('',(20.925,2.4,8.));
#14074=CARTESIAN_POINT('Origin',(21.15,2.9,8.));
#14075=CARTESIAN_POINT('Origin',(19.425,2.4,8.9959292143521));
#14076=CARTESIAN_POINT('',(19.2,2.5,8.9959292143521));
#14077=CARTESIAN_POINT('Origin',(19.425,2.5,8.9959292143521));
#14078=CARTESIAN_POINT('',(19.2,2.9,8.9959292143521));
#14079=CARTESIAN_POINT('',(19.2,2.4,8.9959292143521));
#14080=CARTESIAN_POINT('Origin',(19.425,2.9,8.9959292143521));
#14081=CARTESIAN_POINT('Origin',(19.425,2.4,7.0040707856479));
#14082=CARTESIAN_POINT('',(19.2,2.5,7.0040707856479));
#14083=CARTESIAN_POINT('Origin',(19.425,2.5,7.0040707856479));
#14084=CARTESIAN_POINT('',(19.2,2.9,7.0040707856479));
#14085=CARTESIAN_POINT('',(19.2,2.4,7.0040707856479));
#14086=CARTESIAN_POINT('Origin',(19.425,2.9,7.0040707856479));
#14087=CARTESIAN_POINT('Origin',(20.,2.9,8.));
#14088=CARTESIAN_POINT('',(18.5,2.9,8.));
#14089=CARTESIAN_POINT('Origin',(20.,2.9,8.));
#14090=CARTESIAN_POINT('',(19.5,2.9,8.));
#14091=CARTESIAN_POINT('Origin',(20.,2.9,8.));
#14092=CARTESIAN_POINT('Origin',(20.,2.5,8.));
#14093=CARTESIAN_POINT('',(18.5,2.5,8.));
#14094=CARTESIAN_POINT('Origin',(20.,2.5,8.));
#14095=CARTESIAN_POINT('',(19.5,2.5,8.));
#14096=CARTESIAN_POINT('Origin',(20.,2.5,8.));
#14097=CARTESIAN_POINT('Origin',(20.,2.5,8.));
#14098=CARTESIAN_POINT('',(18.5,2.5,8.));
#14099=CARTESIAN_POINT('Origin',(20.,-1.6,8.));
#14100=CARTESIAN_POINT('',(19.5,-1.6,8.));
#14101=CARTESIAN_POINT('',(19.5,-1.6,8.));
#14102=CARTESIAN_POINT('Origin',(20.,-1.6,8.));
#14103=CARTESIAN_POINT('Origin',(20.,-1.6,8.));
#14104=CARTESIAN_POINT('',(19.5,3.9,8.));
#14105=CARTESIAN_POINT('Origin',(20.,3.9,8.));
#14106=CARTESIAN_POINT('',(19.5,-1.6,8.));
#14107=CARTESIAN_POINT('Origin',(20.,3.9,8.));
#14108=CARTESIAN_POINT('Origin',(20.,-1.6,8.));
#14109=CARTESIAN_POINT('',(0.,0.,0.));
#14110=CARTESIAN_POINT('Origin',(20.,-0.15,8.));
#14111=CARTESIAN_POINT('',(19.495,0.15,8.));
#14112=CARTESIAN_POINT('Origin',(20.,0.15,8.));
#14113=CARTESIAN_POINT('',(19.495,-0.15,8.));
#14114=CARTESIAN_POINT('',(19.495,-0.15,8.));
#14115=CARTESIAN_POINT('Origin',(20.,-0.15,8.));
#14116=CARTESIAN_POINT('Origin',(20.,-0.15,8.));
#14117=CARTESIAN_POINT('',(19.3,0.15,8.));
#14118=CARTESIAN_POINT('Origin',(20.,0.15,8.));
#14119=CARTESIAN_POINT('',(19.3,-0.15,8.));
#14120=CARTESIAN_POINT('',(19.3,-0.15,8.));
#14121=CARTESIAN_POINT('Origin',(20.,-0.15,8.));
#14122=CARTESIAN_POINT('Origin',(20.,0.15,8.));
#14123=CARTESIAN_POINT('Origin',(20.,-0.15,8.));
#14124=CARTESIAN_POINT('',(0.,0.,0.));
#14125=CARTESIAN_POINT('Origin',(20.,1.05,8.));
#14126=CARTESIAN_POINT('',(19.495,2.5,8.));
#14127=CARTESIAN_POINT('Origin',(20.,2.5,8.));
#14128=CARTESIAN_POINT('',(19.495,1.05,8.));
#14129=CARTESIAN_POINT('',(19.495,1.05,8.));
#14130=CARTESIAN_POINT('Origin',(20.,1.05,8.));
#14131=CARTESIAN_POINT('Origin',(20.,1.05,8.));
#14132=CARTESIAN_POINT('',(19.3,2.5,8.));
#14133=CARTESIAN_POINT('Origin',(20.,2.5,8.));
#14134=CARTESIAN_POINT('',(19.3,1.05,8.));
#14135=CARTESIAN_POINT('',(19.3,1.05,8.));
#14136=CARTESIAN_POINT('Origin',(20.,1.05,8.));
#14137=CARTESIAN_POINT('Origin',(20.,2.5,8.));
#14138=CARTESIAN_POINT('Origin',(20.,1.05,8.));
#14139=CARTESIAN_POINT('',(0.,0.,0.));
#14140=CARTESIAN_POINT('Origin',(20.,-1.6,8.));
#14141=CARTESIAN_POINT('',(19.495,-1.05,8.));
#14142=CARTESIAN_POINT('Origin',(20.,-1.05,8.));
#14143=CARTESIAN_POINT('',(19.495,-1.6,8.));
#14144=CARTESIAN_POINT('',(19.495,-1.6,8.));
#14145=CARTESIAN_POINT('Origin',(20.,-1.6,8.));
#14146=CARTESIAN_POINT('Origin',(20.,-1.6,8.));
#14147=CARTESIAN_POINT('',(19.3,-1.05,8.));
#14148=CARTESIAN_POINT('Origin',(20.,-1.05,8.));
#14149=CARTESIAN_POINT('',(19.3,-1.6,8.));
#14150=CARTESIAN_POINT('',(19.3,-1.6,8.));
#14151=CARTESIAN_POINT('Origin',(20.,-1.6,8.));
#14152=CARTESIAN_POINT('Origin',(20.,-1.05,8.));
#14153=CARTESIAN_POINT('Origin',(20.,-1.6,8.));
#14154=CARTESIAN_POINT('',(0.,0.,0.));
#14155=CARTESIAN_POINT('Origin',(20.,-1.8,8.));
#14156=CARTESIAN_POINT('',(19.775,-1.6,8.));
#14157=CARTESIAN_POINT('Origin',(20.,-1.6,8.));
#14158=CARTESIAN_POINT('',(19.775,-1.8,8.));
#14159=CARTESIAN_POINT('',(19.775,-1.8,8.));
#14160=CARTESIAN_POINT('Origin',(20.,-1.8,8.));
#14161=CARTESIAN_POINT('Origin',(20.,-1.8,8.));
#14162=CARTESIAN_POINT('',(19.1,-1.6,8.));
#14163=CARTESIAN_POINT('Origin',(20.,-1.6,8.));
#14164=CARTESIAN_POINT('',(19.1,-1.8,8.));
#14165=CARTESIAN_POINT('',(19.1,-1.8,8.));
#14166=CARTESIAN_POINT('Origin',(20.,-1.8,8.));
#14167=CARTESIAN_POINT('Origin',(20.,-1.6,8.));
#14168=CARTESIAN_POINT('Origin',(20.,-1.8,8.));
#14169=CARTESIAN_POINT('',(0.,0.,0.));
#14170=CARTESIAN_POINT('Origin',(20.,-1.7,14.));
#14171=CARTESIAN_POINT('',(19.835,-1.6,14.));
#14172=CARTESIAN_POINT('Origin',(20.,-1.6,14.));
#14173=CARTESIAN_POINT('',(19.835,0.,14.));
#14174=CARTESIAN_POINT('',(19.835,-1.7,14.));
#14175=CARTESIAN_POINT('Origin',(20.,0.,14.));
#14176=CARTESIAN_POINT('Origin',(20.,0.,14.));
#14177=CARTESIAN_POINT('Origin',(21.15,2.4,14.));
#14178=CARTESIAN_POINT('',(20.925,2.5,14.));
#14179=CARTESIAN_POINT('Origin',(21.15,2.5,14.));
#14180=CARTESIAN_POINT('',(20.925,2.9,14.));
#14181=CARTESIAN_POINT('',(20.925,2.4,14.));
#14182=CARTESIAN_POINT('Origin',(21.15,2.9,14.));
#14183=CARTESIAN_POINT('Origin',(19.425,2.4,14.9959292143521));
#14184=CARTESIAN_POINT('',(19.2,2.5,14.9959292143521));
#14185=CARTESIAN_POINT('Origin',(19.425,2.5,14.9959292143521));
#14186=CARTESIAN_POINT('',(19.2,2.9,14.9959292143521));
#14187=CARTESIAN_POINT('',(19.2,2.4,14.9959292143521));
#14188=CARTESIAN_POINT('Origin',(19.425,2.9,14.9959292143521));
#14189=CARTESIAN_POINT('Origin',(19.425,2.4,13.0040707856479));
#14190=CARTESIAN_POINT('',(19.2,2.5,13.0040707856479));
#14191=CARTESIAN_POINT('Origin',(19.425,2.5,13.0040707856479));
#14192=CARTESIAN_POINT('',(19.2,2.9,13.0040707856479));
#14193=CARTESIAN_POINT('',(19.2,2.4,13.0040707856479));
#14194=CARTESIAN_POINT('Origin',(19.425,2.9,13.0040707856479));
#14195=CARTESIAN_POINT('Origin',(20.,2.9,14.));
#14196=CARTESIAN_POINT('',(18.5,2.9,14.));
#14197=CARTESIAN_POINT('Origin',(20.,2.9,14.));
#14198=CARTESIAN_POINT('',(19.5,2.9,14.));
#14199=CARTESIAN_POINT('Origin',(20.,2.9,14.));
#14200=CARTESIAN_POINT('Origin',(20.,2.5,14.));
#14201=CARTESIAN_POINT('',(18.5,2.5,14.));
#14202=CARTESIAN_POINT('Origin',(20.,2.5,14.));
#14203=CARTESIAN_POINT('',(19.5,2.5,14.));
#14204=CARTESIAN_POINT('Origin',(20.,2.5,14.));
#14205=CARTESIAN_POINT('Origin',(20.,2.5,14.));
#14206=CARTESIAN_POINT('',(18.5,2.5,14.));
#14207=CARTESIAN_POINT('Origin',(20.,-1.6,14.));
#14208=CARTESIAN_POINT('',(19.5,-1.6,14.));
#14209=CARTESIAN_POINT('',(19.5,-1.6,14.));
#14210=CARTESIAN_POINT('Origin',(20.,-1.6,14.));
#14211=CARTESIAN_POINT('Origin',(20.,-1.6,14.));
#14212=CARTESIAN_POINT('',(19.5,3.9,14.));
#14213=CARTESIAN_POINT('Origin',(20.,3.9,14.));
#14214=CARTESIAN_POINT('',(19.5,-1.6,14.));
#14215=CARTESIAN_POINT('Origin',(20.,3.9,14.));
#14216=CARTESIAN_POINT('Origin',(20.,-1.6,14.));
#14217=CARTESIAN_POINT('',(0.,0.,0.));
#14218=CARTESIAN_POINT('Origin',(20.,-0.15,14.));
#14219=CARTESIAN_POINT('',(19.495,0.15,14.));
#14220=CARTESIAN_POINT('Origin',(20.,0.15,14.));
#14221=CARTESIAN_POINT('',(19.495,-0.15,14.));
#14222=CARTESIAN_POINT('',(19.495,-0.15,14.));
#14223=CARTESIAN_POINT('Origin',(20.,-0.15,14.));
#14224=CARTESIAN_POINT('Origin',(20.,-0.15,14.));
#14225=CARTESIAN_POINT('',(19.3,0.15,14.));
#14226=CARTESIAN_POINT('Origin',(20.,0.15,14.));
#14227=CARTESIAN_POINT('',(19.3,-0.15,14.));
#14228=CARTESIAN_POINT('',(19.3,-0.15,14.));
#14229=CARTESIAN_POINT('Origin',(20.,-0.15,14.));
#14230=CARTESIAN_POINT('Origin',(20.,0.15,14.));
#14231=CARTESIAN_POINT('Origin',(20.,-0.15,14.));
#14232=CARTESIAN_POINT('',(0.,0.,0.));
#14233=CARTESIAN_POINT('Origin',(20.,1.05,14.));
#14234=CARTESIAN_POINT('',(19.495,2.5,14.));
#14235=CARTESIAN_POINT('Origin',(20.,2.5,14.));
#14236=CARTESIAN_POINT('',(19.495,1.05,14.));
#14237=CARTESIAN_POINT('',(19.495,1.05,14.));
#14238=CARTESIAN_POINT('Origin',(20.,1.05,14.));
#14239=CARTESIAN_POINT('Origin',(20.,1.05,14.));
#14240=CARTESIAN_POINT('',(19.3,2.5,14.));
#14241=CARTESIAN_POINT('Origin',(20.,2.5,14.));
#14242=CARTESIAN_POINT('',(19.3,1.05,14.));
#14243=CARTESIAN_POINT('',(19.3,1.05,14.));
#14244=CARTESIAN_POINT('Origin',(20.,1.05,14.));
#14245=CARTESIAN_POINT('Origin',(20.,2.5,14.));
#14246=CARTESIAN_POINT('Origin',(20.,1.05,14.));
#14247=CARTESIAN_POINT('',(0.,0.,0.));
#14248=CARTESIAN_POINT('Origin',(20.,-1.6,14.));
#14249=CARTESIAN_POINT('',(19.495,-1.05,14.));
#14250=CARTESIAN_POINT('Origin',(20.,-1.05,14.));
#14251=CARTESIAN_POINT('',(19.495,-1.6,14.));
#14252=CARTESIAN_POINT('',(19.495,-1.6,14.));
#14253=CARTESIAN_POINT('Origin',(20.,-1.6,14.));
#14254=CARTESIAN_POINT('Origin',(20.,-1.6,14.));
#14255=CARTESIAN_POINT('',(19.3,-1.05,14.));
#14256=CARTESIAN_POINT('Origin',(20.,-1.05,14.));
#14257=CARTESIAN_POINT('',(19.3,-1.6,14.));
#14258=CARTESIAN_POINT('',(19.3,-1.6,14.));
#14259=CARTESIAN_POINT('Origin',(20.,-1.6,14.));
#14260=CARTESIAN_POINT('Origin',(20.,-1.05,14.));
#14261=CARTESIAN_POINT('Origin',(20.,-1.6,14.));
#14262=CARTESIAN_POINT('',(0.,0.,0.));
#14263=CARTESIAN_POINT('Origin',(20.,-1.8,14.));
#14264=CARTESIAN_POINT('',(19.775,-1.6,14.));
#14265=CARTESIAN_POINT('Origin',(20.,-1.6,14.));
#14266=CARTESIAN_POINT('',(19.775,-1.8,14.));
#14267=CARTESIAN_POINT('',(19.775,-1.8,14.));
#14268=CARTESIAN_POINT('Origin',(20.,-1.8,14.));
#14269=CARTESIAN_POINT('Origin',(20.,-1.8,14.));
#14270=CARTESIAN_POINT('',(19.1,-1.6,14.));
#14271=CARTESIAN_POINT('Origin',(20.,-1.6,14.));
#14272=CARTESIAN_POINT('',(19.1,-1.8,14.));
#14273=CARTESIAN_POINT('',(19.1,-1.8,14.));
#14274=CARTESIAN_POINT('Origin',(20.,-1.8,14.));
#14275=CARTESIAN_POINT('Origin',(20.,-1.6,14.));
#14276=CARTESIAN_POINT('Origin',(20.,-1.8,14.));
#14277=CARTESIAN_POINT('',(0.,0.,0.));
#14278=CARTESIAN_POINT('Origin',(0.3,0.4,0.));
#14279=CARTESIAN_POINT('',(-0.3,0.4,-3.67394039744206E-17));
#14280=CARTESIAN_POINT('Origin',(0.,0.4,0.));
#14281=CARTESIAN_POINT('Origin',(0.,0.375,0.));
#14282=CARTESIAN_POINT('',(-0.35,0.35,-4.28626379701573E-17));
#14283=CARTESIAN_POINT('Origin',(0.,0.35,0.));
#14284=CARTESIAN_POINT('',(-0.325,0.375,-3.9801020972289E-17));
#14285=CARTESIAN_POINT('Origin',(0.,0.19,0.));
#14286=CARTESIAN_POINT('',(-0.35,0.03,-4.28626379701574E-17));
#14287=CARTESIAN_POINT('Origin',(0.,0.03,0.));
#14288=CARTESIAN_POINT('',(-0.35,0.19,-4.28626379701574E-17));
#14289=CARTESIAN_POINT('Origin',(0.,0.0149999999999999,0.));
#14290=CARTESIAN_POINT('',(-0.32,-3.29597460435593E-17,-3.91886975727153E-17));
#14291=CARTESIAN_POINT('Origin',(0.,0.,0.));
#14292=CARTESIAN_POINT('',(-0.335,0.0149999999999999,-4.10256677714363E-17));
#14293=CARTESIAN_POINT('Origin',(0.22,0.,0.));
#14294=CARTESIAN_POINT('',(-0.22,-6.93889390390723E-18,-2.69422295812418E-17));
#14295=CARTESIAN_POINT('Origin',(0.,0.,0.));
#14296=CARTESIAN_POINT('Origin',(0.,-0.02,0.));
#14297=CARTESIAN_POINT('',(-0.1954,-0.0492,2.39295984553393E-17));
#14298=CARTESIAN_POINT('Origin',(0.,-0.0492,0.));
#14299=CARTESIAN_POINT('',(-0.21,-0.02,-2.57175827820944E-17));
#14300=CARTESIAN_POINT('Origin',(0.,-0.8,0.));
#14301=CARTESIAN_POINT('',(-0.1954,-1.5646,2.39295984553393E-17));
#14302=CARTESIAN_POINT('Origin',(0.,-1.5646,0.));
#14303=CARTESIAN_POINT('',(-0.1954,-0.8,-2.39295984553393E-17));
#14304=CARTESIAN_POINT('Origin',(0.,-1.58,0.));
#14305=CARTESIAN_POINT('',(-0.16,-1.6,-1.95943487863577E-17));
#14306=CARTESIAN_POINT('Origin',(0.,-1.6,0.));
#14307=CARTESIAN_POINT('',(-0.18,-1.58,-2.20436423846524E-17));
#14308=CARTESIAN_POINT('Origin',(0.,-1.6,0.));
#14309=CARTESIAN_POINT('Origin',(0.0866025403784439,-0.4,-0.15));
#14310=CARTESIAN_POINT('',(0.173205080756888,-0.4,0.));
#14311=CARTESIAN_POINT('',(0.0866025403784439,-0.4,-0.15));
#14312=CARTESIAN_POINT('',(0.173205080756888,-0.4,0.));
#14313=CARTESIAN_POINT('',(0.0866025403784439,-0.64,-0.15));
#14314=CARTESIAN_POINT('',(0.0866025403784439,-0.4,-0.15));
#14315=CARTESIAN_POINT('',(0.173205080756888,-0.64,0.));
#14316=CARTESIAN_POINT('',(0.173205080756888,-0.64,0.));
#14317=CARTESIAN_POINT('',(0.173205080756888,-0.4,0.));
#14318=CARTESIAN_POINT('Origin',(-0.0866025403784438,-0.4,-0.15));
#14319=CARTESIAN_POINT('',(-0.0866025403784438,-0.4,-0.15));
#14320=CARTESIAN_POINT('',(0.0866025403784439,-0.4,-0.15));
#14321=CARTESIAN_POINT('',(-0.0866025403784438,-0.64,-0.15));
#14322=CARTESIAN_POINT('',(-0.0866025403784438,-0.4,-0.15));
#14323=CARTESIAN_POINT('',(0.0866025403784439,-0.64,-0.15));
#14324=CARTESIAN_POINT('Origin',(-0.173205080756888,-0.4,-2.77555756156289E-17));
#14325=CARTESIAN_POINT('',(-0.173205080756888,-0.4,-2.12115047744981E-17));
#14326=CARTESIAN_POINT('',(-0.0866025403784438,-0.4,-0.15));
#14327=CARTESIAN_POINT('',(-0.173205080756888,-0.64,-2.77555756156289E-17));
#14328=CARTESIAN_POINT('',(-0.173205080756888,-0.4,-2.12115047744981E-17));
#14329=CARTESIAN_POINT('',(-0.0866025403784438,-0.64,-0.15));
#14330=CARTESIAN_POINT('Origin',(-0.0866025403784439,-0.4,0.15));
#14331=CARTESIAN_POINT('',(-0.0866025403784439,-0.4,0.15));
#14332=CARTESIAN_POINT('',(-0.173205080756888,-0.4,-2.12115047744981E-17));
#14333=CARTESIAN_POINT('',(-0.0866025403784439,-0.64,0.15));
#14334=CARTESIAN_POINT('',(-0.0866025403784439,-0.4,0.15));
#14335=CARTESIAN_POINT('',(-0.173205080756888,-0.64,-2.12115047744981E-17));
#14336=CARTESIAN_POINT('Origin',(0.0866025403784439,-0.4,0.15));
#14337=CARTESIAN_POINT('',(0.0866025403784439,-0.4,0.15));
#14338=CARTESIAN_POINT('',(-0.0866025403784439,-0.4,0.15));
#14339=CARTESIAN_POINT('',(0.0866025403784439,-0.64,0.15));
#14340=CARTESIAN_POINT('',(0.0866025403784439,-0.4,0.15));
#14341=CARTESIAN_POINT('',(-0.0866025403784439,-0.64,0.15));
#14342=CARTESIAN_POINT('Origin',(0.173205080756888,-0.4,0.));
#14343=CARTESIAN_POINT('',(0.0866025403784439,-0.4,0.15));
#14344=CARTESIAN_POINT('',(0.0866025403784439,-0.64,0.15));
#14345=CARTESIAN_POINT('Origin',(0.,-0.4,-2.77555756156289E-17));
#14346=CARTESIAN_POINT('Origin',(0.,-0.64,-2.77555756156289E-17));
#14347=CARTESIAN_POINT('',(0.,0.,0.));
#14348=CARTESIAN_POINT('',(0.,0.,0.));
#14349=CARTESIAN_POINT('',(0.,0.,0.));
#14350=CARTESIAN_POINT('',(0.,0.,0.));
#14351=CARTESIAN_POINT('',(0.,0.,0.));
#14352=CARTESIAN_POINT('',(0.,0.,0.));
#14353=CARTESIAN_POINT('',(0.,0.,0.));
#14354=CARTESIAN_POINT('',(0.,0.,0.));
#14355=CARTESIAN_POINT('',(0.,0.,0.));
#14356=CARTESIAN_POINT('',(0.,0.,0.));
#14357=CARTESIAN_POINT('',(0.,0.,0.));
#14358=CARTESIAN_POINT('',(0.,0.,0.));
#14359=CARTESIAN_POINT('',(0.,0.,0.));
#14360=CARTESIAN_POINT('',(0.,0.,0.));
#14361=CARTESIAN_POINT('',(0.,0.,0.));
#14362=CARTESIAN_POINT('',(0.,0.,0.));
#14363=CARTESIAN_POINT('',(-3.2,3.5,1.8));
#14364=CARTESIAN_POINT('',(-3.2,5.5,1.8));
#14365=CARTESIAN_POINT('',(3.2,3.5,1.8));
#14366=CARTESIAN_POINT('',(3.2,5.5,1.8));
#14367=CARTESIAN_POINT('',(1.15,2.5,8.));
#14368=CARTESIAN_POINT('',(-0.575,2.5,8.9959292143521));
#14369=CARTESIAN_POINT('',(-0.575000000000001,2.5,7.0040707856479));
#14370=CARTESIAN_POINT('',(-2.22044604925031E-16,-4.2,8.));
#14371=CARTESIAN_POINT('',(1.15,2.5,14.));
#14372=CARTESIAN_POINT('',(-0.575,2.5,14.9959292143521));
#14373=CARTESIAN_POINT('',(-0.575000000000001,2.5,13.0040707856479));
#14374=CARTESIAN_POINT('',(0.,-1.8,14.));
#14375=CARTESIAN_POINT('',(-3.5,3.4,11.));
#14376=CARTESIAN_POINT('',(0.,0.,0.));
#14377=CARTESIAN_POINT('',(0.,0.,0.));
#14378=CARTESIAN_POINT('',(0.,0.,0.));
#14379=CARTESIAN_POINT('',(0.,0.,0.));
#14380=CARTESIAN_POINT('',(0.,0.,0.));
#14381=CARTESIAN_POINT('',(0.,0.,0.));
#14382=CARTESIAN_POINT('',(0.,0.,0.));
#14383=CARTESIAN_POINT('',(0.,0.,0.));
#14384=CARTESIAN_POINT('',(0.,0.,0.));
#14385=CARTESIAN_POINT('',(0.,0.,0.));
#14386=CARTESIAN_POINT('',(0.,0.,0.));
#14387=CARTESIAN_POINT('',(21.15,2.5,8.));
#14388=CARTESIAN_POINT('',(19.425,2.5,8.9959292143521));
#14389=CARTESIAN_POINT('',(19.425,2.5,7.0040707856479));
#14390=CARTESIAN_POINT('',(20.,-1.8,8.));
#14391=CARTESIAN_POINT('',(21.15,2.5,14.));
#14392=CARTESIAN_POINT('',(19.425,2.5,14.9959292143521));
#14393=CARTESIAN_POINT('',(19.425,2.5,13.0040707856479));
#14394=CARTESIAN_POINT('',(20.,-1.8,14.));
#14395=CARTESIAN_POINT('',(0.,0.,0.));
#14396=CARTESIAN_POINT('',(0.,0.,0.));
#14397=CARTESIAN_POINT('',(0.,0.,0.));
#14398=CARTESIAN_POINT('',(0.,0.,0.));
#14399=UNCERTAINTY_MEASURE_WITH_UNIT(LENGTH_MEASURE(0.001),#14513,
'DISTANCE_ACCURACY_VALUE',
'Maximum model space distance between geometric entities at asserted c
onnectivities');
#14400=UNCERTAINTY_MEASURE_WITH_UNIT(LENGTH_MEASURE(0.001),#14513,
'DISTANCE_ACCURACY_VALUE',
'Maximum model space distance between geometric entities at asserted c
onnectivities');
#14401=UNCERTAINTY_MEASURE_WITH_UNIT(LENGTH_MEASURE(0.001),#14513,
'DISTANCE_ACCURACY_VALUE',
'Maximum model space distance between geometric entities at asserted c
onnectivities');
#14402=UNCERTAINTY_MEASURE_WITH_UNIT(LENGTH_MEASURE(0.001),#14513,
'DISTANCE_ACCURACY_VALUE',
'Maximum model space distance between geometric entities at asserted c
onnectivities');
#14403=UNCERTAINTY_MEASURE_WITH_UNIT(LENGTH_MEASURE(0.001),#14513,
'DISTANCE_ACCURACY_VALUE',
'Maximum model space distance between geometric entities at asserted c
onnectivities');
#14404=UNCERTAINTY_MEASURE_WITH_UNIT(LENGTH_MEASURE(0.001),#14513,
'DISTANCE_ACCURACY_VALUE',
'Maximum model space distance between geometric entities at asserted c
onnectivities');
#14405=UNCERTAINTY_MEASURE_WITH_UNIT(LENGTH_MEASURE(0.001),#14513,
'DISTANCE_ACCURACY_VALUE',
'Maximum model space distance between geometric entities at asserted c
onnectivities');
#14406=UNCERTAINTY_MEASURE_WITH_UNIT(LENGTH_MEASURE(0.001),#14513,
'DISTANCE_ACCURACY_VALUE',
'Maximum model space distance between geometric entities at asserted c
onnectivities');
#14407=UNCERTAINTY_MEASURE_WITH_UNIT(LENGTH_MEASURE(0.001),#14513,
'DISTANCE_ACCURACY_VALUE',
'Maximum model space distance between geometric entities at asserted c
onnectivities');
#14408=UNCERTAINTY_MEASURE_WITH_UNIT(LENGTH_MEASURE(0.001),#14513,
'DISTANCE_ACCURACY_VALUE',
'Maximum model space distance between geometric entities at asserted c
onnectivities');
#14409=UNCERTAINTY_MEASURE_WITH_UNIT(LENGTH_MEASURE(0.001),#14513,
'DISTANCE_ACCURACY_VALUE',
'Maximum model space distance between geometric entities at asserted c
onnectivities');
#14410=UNCERTAINTY_MEASURE_WITH_UNIT(LENGTH_MEASURE(0.001),#14513,
'DISTANCE_ACCURACY_VALUE',
'Maximum model space distance between geometric entities at asserted c
onnectivities');
#14411=UNCERTAINTY_MEASURE_WITH_UNIT(LENGTH_MEASURE(0.001),#14513,
'DISTANCE_ACCURACY_VALUE',
'Maximum model space distance between geometric entities at asserted c
onnectivities');
#14412=UNCERTAINTY_MEASURE_WITH_UNIT(LENGTH_MEASURE(0.001),#14513,
'DISTANCE_ACCURACY_VALUE',
'Maximum model space distance between geometric entities at asserted c
onnectivities');
#14413=UNCERTAINTY_MEASURE_WITH_UNIT(LENGTH_MEASURE(0.001),#14513,
'DISTANCE_ACCURACY_VALUE',
'Maximum model space distance between geometric entities at asserted c
onnectivities');
#14414=UNCERTAINTY_MEASURE_WITH_UNIT(LENGTH_MEASURE(0.001),#14513,
'DISTANCE_ACCURACY_VALUE',
'Maximum model space distance between geometric entities at asserted c
onnectivities');
#14415=UNCERTAINTY_MEASURE_WITH_UNIT(LENGTH_MEASURE(0.001),#14513,
'DISTANCE_ACCURACY_VALUE',
'Maximum model space distance between geometric entities at asserted c
onnectivities');
#14416=UNCERTAINTY_MEASURE_WITH_UNIT(LENGTH_MEASURE(0.001),#14513,
'DISTANCE_ACCURACY_VALUE',
'Maximum model space distance between geometric entities at asserted c
onnectivities');
#14417=UNCERTAINTY_MEASURE_WITH_UNIT(LENGTH_MEASURE(0.001),#14513,
'DISTANCE_ACCURACY_VALUE',
'Maximum model space distance between geometric entities at asserted c
onnectivities');
#14418=UNCERTAINTY_MEASURE_WITH_UNIT(LENGTH_MEASURE(0.001),#14513,
'DISTANCE_ACCURACY_VALUE',
'Maximum model space distance between geometric entities at asserted c
onnectivities');
#14419=UNCERTAINTY_MEASURE_WITH_UNIT(LENGTH_MEASURE(0.001),#14513,
'DISTANCE_ACCURACY_VALUE',
'Maximum model space distance between geometric entities at asserted c
onnectivities');
#14420=UNCERTAINTY_MEASURE_WITH_UNIT(LENGTH_MEASURE(0.001),#14513,
'DISTANCE_ACCURACY_VALUE',
'Maximum model space distance between geometric entities at asserted c
onnectivities');
#14421=UNCERTAINTY_MEASURE_WITH_UNIT(LENGTH_MEASURE(0.001),#14513,
'DISTANCE_ACCURACY_VALUE',
'Maximum model space distance between geometric entities at asserted c
onnectivities');
#14422=UNCERTAINTY_MEASURE_WITH_UNIT(LENGTH_MEASURE(0.001),#14513,
'DISTANCE_ACCURACY_VALUE',
'Maximum model space distance between geometric entities at asserted c
onnectivities');
#14423=UNCERTAINTY_MEASURE_WITH_UNIT(LENGTH_MEASURE(0.001),#14513,
'DISTANCE_ACCURACY_VALUE',
'Maximum model space distance between geometric entities at asserted c
onnectivities');
#14424=UNCERTAINTY_MEASURE_WITH_UNIT(LENGTH_MEASURE(0.001),#14513,
'DISTANCE_ACCURACY_VALUE',
'Maximum model space distance between geometric entities at asserted c
onnectivities');
#14425=UNCERTAINTY_MEASURE_WITH_UNIT(LENGTH_MEASURE(0.001),#14513,
'DISTANCE_ACCURACY_VALUE',
'Maximum model space distance between geometric entities at asserted c
onnectivities');
#14426=UNCERTAINTY_MEASURE_WITH_UNIT(LENGTH_MEASURE(0.001),#14513,
'DISTANCE_ACCURACY_VALUE',
'Maximum model space distance between geometric entities at asserted c
onnectivities');
#14427=UNCERTAINTY_MEASURE_WITH_UNIT(LENGTH_MEASURE(0.001),#14513,
'DISTANCE_ACCURACY_VALUE',
'Maximum model space distance between geometric entities at asserted c
onnectivities');
#14428=UNCERTAINTY_MEASURE_WITH_UNIT(LENGTH_MEASURE(0.001),#14513,
'DISTANCE_ACCURACY_VALUE',
'Maximum model space distance between geometric entities at asserted c
onnectivities');
#14429=UNCERTAINTY_MEASURE_WITH_UNIT(LENGTH_MEASURE(0.001),#14513,
'DISTANCE_ACCURACY_VALUE',
'Maximum model space distance between geometric entities at asserted c
onnectivities');
#14430=UNCERTAINTY_MEASURE_WITH_UNIT(LENGTH_MEASURE(0.001),#14513,
'DISTANCE_ACCURACY_VALUE',
'Maximum model space distance between geometric entities at asserted c
onnectivities');
#14431=UNCERTAINTY_MEASURE_WITH_UNIT(LENGTH_MEASURE(0.001),#14513,
'DISTANCE_ACCURACY_VALUE',
'Maximum model space distance between geometric entities at asserted c
onnectivities');
#14432=UNCERTAINTY_MEASURE_WITH_UNIT(LENGTH_MEASURE(0.001),#14513,
'DISTANCE_ACCURACY_VALUE',
'Maximum model space distance between geometric entities at asserted c
onnectivities');
#14433=UNCERTAINTY_MEASURE_WITH_UNIT(LENGTH_MEASURE(0.001),#14513,
'DISTANCE_ACCURACY_VALUE',
'Maximum model space distance between geometric entities at asserted c
onnectivities');
#14434=UNCERTAINTY_MEASURE_WITH_UNIT(LENGTH_MEASURE(0.001),#14513,
'DISTANCE_ACCURACY_VALUE',
'Maximum model space distance between geometric entities at asserted c
onnectivities');
#14435=UNCERTAINTY_MEASURE_WITH_UNIT(LENGTH_MEASURE(0.001),#14513,
'DISTANCE_ACCURACY_VALUE',
'Maximum model space distance between geometric entities at asserted c
onnectivities');
#14436=UNCERTAINTY_MEASURE_WITH_UNIT(LENGTH_MEASURE(0.001),#14513,
'DISTANCE_ACCURACY_VALUE',
'Maximum model space distance between geometric entities at asserted c
onnectivities');
#14437=UNCERTAINTY_MEASURE_WITH_UNIT(LENGTH_MEASURE(0.001),#14513,
'DISTANCE_ACCURACY_VALUE',
'Maximum model space distance between geometric entities at asserted c
onnectivities');
#14438=UNCERTAINTY_MEASURE_WITH_UNIT(LENGTH_MEASURE(0.001),#14513,
'DISTANCE_ACCURACY_VALUE',
'Maximum model space distance between geometric entities at asserted c
onnectivities');
#14439=UNCERTAINTY_MEASURE_WITH_UNIT(LENGTH_MEASURE(0.001),#14513,
'DISTANCE_ACCURACY_VALUE',
'Maximum model space distance between geometric entities at asserted c
onnectivities');
#14440=UNCERTAINTY_MEASURE_WITH_UNIT(LENGTH_MEASURE(0.001),#14513,
'DISTANCE_ACCURACY_VALUE',
'Maximum model space distance between geometric entities at asserted c
onnectivities');
#14441=UNCERTAINTY_MEASURE_WITH_UNIT(LENGTH_MEASURE(0.001),#14513,
'DISTANCE_ACCURACY_VALUE',
'Maximum model space distance between geometric entities at asserted c
onnectivities');
#14442=UNCERTAINTY_MEASURE_WITH_UNIT(LENGTH_MEASURE(0.001),#14513,
'DISTANCE_ACCURACY_VALUE',
'Maximum model space distance between geometric entities at asserted c
onnectivities');
#14443=UNCERTAINTY_MEASURE_WITH_UNIT(LENGTH_MEASURE(0.001),#14513,
'DISTANCE_ACCURACY_VALUE',
'Maximum model space distance between geometric entities at asserted c
onnectivities');
#14444=UNCERTAINTY_MEASURE_WITH_UNIT(LENGTH_MEASURE(0.001),#14513,
'DISTANCE_ACCURACY_VALUE',
'Maximum model space distance between geometric entities at asserted c
onnectivities');
#14445=UNCERTAINTY_MEASURE_WITH_UNIT(LENGTH_MEASURE(0.001),#14513,
'DISTANCE_ACCURACY_VALUE',
'Maximum model space distance between geometric entities at asserted c
onnectivities');
#14446=UNCERTAINTY_MEASURE_WITH_UNIT(LENGTH_MEASURE(0.001),#14513,
'DISTANCE_ACCURACY_VALUE',
'Maximum model space distance between geometric entities at asserted c
onnectivities');
#14447=UNCERTAINTY_MEASURE_WITH_UNIT(LENGTH_MEASURE(0.001),#14513,
'DISTANCE_ACCURACY_VALUE',
'Maximum model space distance between geometric entities at asserted c
onnectivities');
#14448=UNCERTAINTY_MEASURE_WITH_UNIT(LENGTH_MEASURE(0.001),#14513,
'DISTANCE_ACCURACY_VALUE',
'Maximum model space distance between geometric entities at asserted c
onnectivities');
#14449=UNCERTAINTY_MEASURE_WITH_UNIT(LENGTH_MEASURE(0.001),#14513,
'DISTANCE_ACCURACY_VALUE',
'Maximum model space distance between geometric entities at asserted c
onnectivities');
#14450=UNCERTAINTY_MEASURE_WITH_UNIT(LENGTH_MEASURE(0.001),#14513,
'DISTANCE_ACCURACY_VALUE',
'Maximum model space distance between geometric entities at asserted c
onnectivities');
#14451=UNCERTAINTY_MEASURE_WITH_UNIT(LENGTH_MEASURE(0.001),#14513,
'DISTANCE_ACCURACY_VALUE',
'Maximum model space distance between geometric entities at asserted c
onnectivities');
#14452=UNCERTAINTY_MEASURE_WITH_UNIT(LENGTH_MEASURE(0.001),#14513,
'DISTANCE_ACCURACY_VALUE',
'Maximum model space distance between geometric entities at asserted c
onnectivities');
#14453=UNCERTAINTY_MEASURE_WITH_UNIT(LENGTH_MEASURE(0.001),#14513,
'DISTANCE_ACCURACY_VALUE',
'Maximum model space distance between geometric entities at asserted c
onnectivities');
#14454=UNCERTAINTY_MEASURE_WITH_UNIT(LENGTH_MEASURE(0.001),#14513,
'DISTANCE_ACCURACY_VALUE',
'Maximum model space distance between geometric entities at asserted c
onnectivities');
#14455=UNCERTAINTY_MEASURE_WITH_UNIT(LENGTH_MEASURE(0.001),#14513,
'DISTANCE_ACCURACY_VALUE',
'Maximum model space distance between geometric entities at asserted c
onnectivities');
#14456=(
GEOMETRIC_REPRESENTATION_CONTEXT(3)
GLOBAL_UNCERTAINTY_ASSIGNED_CONTEXT((#14399))
GLOBAL_UNIT_ASSIGNED_CONTEXT((#14513,#14515,#14516))
REPRESENTATION_CONTEXT('','3D')
);
#14457=(
GEOMETRIC_REPRESENTATION_CONTEXT(3)
GLOBAL_UNCERTAINTY_ASSIGNED_CONTEXT((#14400))
GLOBAL_UNIT_ASSIGNED_CONTEXT((#14513,#14515,#14516))
REPRESENTATION_CONTEXT('','3D')
);
#14458=(
GEOMETRIC_REPRESENTATION_CONTEXT(3)
GLOBAL_UNCERTAINTY_ASSIGNED_CONTEXT((#14401))
GLOBAL_UNIT_ASSIGNED_CONTEXT((#14513,#14515,#14516))
REPRESENTATION_CONTEXT('','3D')
);
#14459=(
GEOMETRIC_REPRESENTATION_CONTEXT(3)
GLOBAL_UNCERTAINTY_ASSIGNED_CONTEXT((#14402))
GLOBAL_UNIT_ASSIGNED_CONTEXT((#14513,#14515,#14516))
REPRESENTATION_CONTEXT('','3D')
);
#14460=(
GEOMETRIC_REPRESENTATION_CONTEXT(3)
GLOBAL_UNCERTAINTY_ASSIGNED_CONTEXT((#14403))
GLOBAL_UNIT_ASSIGNED_CONTEXT((#14513,#14515,#14516))
REPRESENTATION_CONTEXT('','3D')
);
#14461=(
GEOMETRIC_REPRESENTATION_CONTEXT(3)
GLOBAL_UNCERTAINTY_ASSIGNED_CONTEXT((#14404))
GLOBAL_UNIT_ASSIGNED_CONTEXT((#14513,#14515,#14516))
REPRESENTATION_CONTEXT('','3D')
);
#14462=(
GEOMETRIC_REPRESENTATION_CONTEXT(3)
GLOBAL_UNCERTAINTY_ASSIGNED_CONTEXT((#14405))
GLOBAL_UNIT_ASSIGNED_CONTEXT((#14513,#14515,#14516))
REPRESENTATION_CONTEXT('','3D')
);
#14463=(
GEOMETRIC_REPRESENTATION_CONTEXT(3)
GLOBAL_UNCERTAINTY_ASSIGNED_CONTEXT((#14406))
GLOBAL_UNIT_ASSIGNED_CONTEXT((#14513,#14515,#14516))
REPRESENTATION_CONTEXT('','3D')
);
#14464=(
GEOMETRIC_REPRESENTATION_CONTEXT(3)
GLOBAL_UNCERTAINTY_ASSIGNED_CONTEXT((#14407))
GLOBAL_UNIT_ASSIGNED_CONTEXT((#14513,#14515,#14516))
REPRESENTATION_CONTEXT('','3D')
);
#14465=(
GEOMETRIC_REPRESENTATION_CONTEXT(3)
GLOBAL_UNCERTAINTY_ASSIGNED_CONTEXT((#14408))
GLOBAL_UNIT_ASSIGNED_CONTEXT((#14513,#14515,#14516))
REPRESENTATION_CONTEXT('','3D')
);
#14466=(
GEOMETRIC_REPRESENTATION_CONTEXT(3)
GLOBAL_UNCERTAINTY_ASSIGNED_CONTEXT((#14409))
GLOBAL_UNIT_ASSIGNED_CONTEXT((#14513,#14515,#14516))
REPRESENTATION_CONTEXT('','3D')
);
#14467=(
GEOMETRIC_REPRESENTATION_CONTEXT(3)
GLOBAL_UNCERTAINTY_ASSIGNED_CONTEXT((#14410))
GLOBAL_UNIT_ASSIGNED_CONTEXT((#14513,#14515,#14516))
REPRESENTATION_CONTEXT('','3D')
);
#14468=(
GEOMETRIC_REPRESENTATION_CONTEXT(3)
GLOBAL_UNCERTAINTY_ASSIGNED_CONTEXT((#14411))
GLOBAL_UNIT_ASSIGNED_CONTEXT((#14513,#14515,#14516))
REPRESENTATION_CONTEXT('','3D')
);
#14469=(
GEOMETRIC_REPRESENTATION_CONTEXT(3)
GLOBAL_UNCERTAINTY_ASSIGNED_CONTEXT((#14412))
GLOBAL_UNIT_ASSIGNED_CONTEXT((#14513,#14515,#14516))
REPRESENTATION_CONTEXT('','3D')
);
#14470=(
GEOMETRIC_REPRESENTATION_CONTEXT(3)
GLOBAL_UNCERTAINTY_ASSIGNED_CONTEXT((#14413))
GLOBAL_UNIT_ASSIGNED_CONTEXT((#14513,#14515,#14516))
REPRESENTATION_CONTEXT('','3D')
);
#14471=(
GEOMETRIC_REPRESENTATION_CONTEXT(3)
GLOBAL_UNCERTAINTY_ASSIGNED_CONTEXT((#14414))
GLOBAL_UNIT_ASSIGNED_CONTEXT((#14513,#14515,#14516))
REPRESENTATION_CONTEXT('','3D')
);
#14472=(
GEOMETRIC_REPRESENTATION_CONTEXT(3)
GLOBAL_UNCERTAINTY_ASSIGNED_CONTEXT((#14415))
GLOBAL_UNIT_ASSIGNED_CONTEXT((#14513,#14515,#14516))
REPRESENTATION_CONTEXT('','3D')
);
#14473=(
GEOMETRIC_REPRESENTATION_CONTEXT(3)
GLOBAL_UNCERTAINTY_ASSIGNED_CONTEXT((#14416))
GLOBAL_UNIT_ASSIGNED_CONTEXT((#14513,#14515,#14516))
REPRESENTATION_CONTEXT('','3D')
);
#14474=(
GEOMETRIC_REPRESENTATION_CONTEXT(3)
GLOBAL_UNCERTAINTY_ASSIGNED_CONTEXT((#14417))
GLOBAL_UNIT_ASSIGNED_CONTEXT((#14513,#14515,#14516))
REPRESENTATION_CONTEXT('','3D')
);
#14475=(
GEOMETRIC_REPRESENTATION_CONTEXT(3)
GLOBAL_UNCERTAINTY_ASSIGNED_CONTEXT((#14418))
GLOBAL_UNIT_ASSIGNED_CONTEXT((#14513,#14515,#14516))
REPRESENTATION_CONTEXT('','3D')
);
#14476=(
GEOMETRIC_REPRESENTATION_CONTEXT(3)
GLOBAL_UNCERTAINTY_ASSIGNED_CONTEXT((#14419))
GLOBAL_UNIT_ASSIGNED_CONTEXT((#14513,#14515,#14516))
REPRESENTATION_CONTEXT('','3D')
);
#14477=(
GEOMETRIC_REPRESENTATION_CONTEXT(3)
GLOBAL_UNCERTAINTY_ASSIGNED_CONTEXT((#14420))
GLOBAL_UNIT_ASSIGNED_CONTEXT((#14513,#14515,#14516))
REPRESENTATION_CONTEXT('','3D')
);
#14478=(
GEOMETRIC_REPRESENTATION_CONTEXT(3)
GLOBAL_UNCERTAINTY_ASSIGNED_CONTEXT((#14421))
GLOBAL_UNIT_ASSIGNED_CONTEXT((#14513,#14515,#14516))
REPRESENTATION_CONTEXT('','3D')
);
#14479=(
GEOMETRIC_REPRESENTATION_CONTEXT(3)
GLOBAL_UNCERTAINTY_ASSIGNED_CONTEXT((#14422))
GLOBAL_UNIT_ASSIGNED_CONTEXT((#14513,#14515,#14516))
REPRESENTATION_CONTEXT('','3D')
);
#14480=(
GEOMETRIC_REPRESENTATION_CONTEXT(3)
GLOBAL_UNCERTAINTY_ASSIGNED_CONTEXT((#14423))
GLOBAL_UNIT_ASSIGNED_CONTEXT((#14513,#14515,#14516))
REPRESENTATION_CONTEXT('','3D')
);
#14481=(
GEOMETRIC_REPRESENTATION_CONTEXT(3)
GLOBAL_UNCERTAINTY_ASSIGNED_CONTEXT((#14424))
GLOBAL_UNIT_ASSIGNED_CONTEXT((#14513,#14515,#14516))
REPRESENTATION_CONTEXT('','3D')
);
#14482=(
GEOMETRIC_REPRESENTATION_CONTEXT(3)
GLOBAL_UNCERTAINTY_ASSIGNED_CONTEXT((#14425))
GLOBAL_UNIT_ASSIGNED_CONTEXT((#14513,#14515,#14516))
REPRESENTATION_CONTEXT('','3D')
);
#14483=(
GEOMETRIC_REPRESENTATION_CONTEXT(3)
GLOBAL_UNCERTAINTY_ASSIGNED_CONTEXT((#14426))
GLOBAL_UNIT_ASSIGNED_CONTEXT((#14513,#14515,#14516))
REPRESENTATION_CONTEXT('','3D')
);
#14484=(
GEOMETRIC_REPRESENTATION_CONTEXT(3)
GLOBAL_UNCERTAINTY_ASSIGNED_CONTEXT((#14427))
GLOBAL_UNIT_ASSIGNED_CONTEXT((#14513,#14515,#14516))
REPRESENTATION_CONTEXT('','3D')
);
#14485=(
GEOMETRIC_REPRESENTATION_CONTEXT(3)
GLOBAL_UNCERTAINTY_ASSIGNED_CONTEXT((#14428))
GLOBAL_UNIT_ASSIGNED_CONTEXT((#14513,#14515,#14516))
REPRESENTATION_CONTEXT('','3D')
);
#14486=(
GEOMETRIC_REPRESENTATION_CONTEXT(3)
GLOBAL_UNCERTAINTY_ASSIGNED_CONTEXT((#14429))
GLOBAL_UNIT_ASSIGNED_CONTEXT((#14513,#14515,#14516))
REPRESENTATION_CONTEXT('','3D')
);
#14487=(
GEOMETRIC_REPRESENTATION_CONTEXT(3)
GLOBAL_UNCERTAINTY_ASSIGNED_CONTEXT((#14430))
GLOBAL_UNIT_ASSIGNED_CONTEXT((#14513,#14515,#14516))
REPRESENTATION_CONTEXT('','3D')
);
#14488=(
GEOMETRIC_REPRESENTATION_CONTEXT(3)
GLOBAL_UNCERTAINTY_ASSIGNED_CONTEXT((#14431))
GLOBAL_UNIT_ASSIGNED_CONTEXT((#14513,#14515,#14516))
REPRESENTATION_CONTEXT('','3D')
);
#14489=(
GEOMETRIC_REPRESENTATION_CONTEXT(3)
GLOBAL_UNCERTAINTY_ASSIGNED_CONTEXT((#14432))
GLOBAL_UNIT_ASSIGNED_CONTEXT((#14513,#14515,#14516))
REPRESENTATION_CONTEXT('','3D')
);
#14490=(
GEOMETRIC_REPRESENTATION_CONTEXT(3)
GLOBAL_UNCERTAINTY_ASSIGNED_CONTEXT((#14433))
GLOBAL_UNIT_ASSIGNED_CONTEXT((#14513,#14515,#14516))
REPRESENTATION_CONTEXT('','3D')
);
#14491=(
GEOMETRIC_REPRESENTATION_CONTEXT(3)
GLOBAL_UNCERTAINTY_ASSIGNED_CONTEXT((#14434))
GLOBAL_UNIT_ASSIGNED_CONTEXT((#14513,#14515,#14516))
REPRESENTATION_CONTEXT('','3D')
);
#14492=(
GEOMETRIC_REPRESENTATION_CONTEXT(3)
GLOBAL_UNCERTAINTY_ASSIGNED_CONTEXT((#14435))
GLOBAL_UNIT_ASSIGNED_CONTEXT((#14513,#14515,#14516))
REPRESENTATION_CONTEXT('','3D')
);
#14493=(
GEOMETRIC_REPRESENTATION_CONTEXT(3)
GLOBAL_UNCERTAINTY_ASSIGNED_CONTEXT((#14436))
GLOBAL_UNIT_ASSIGNED_CONTEXT((#14513,#14515,#14516))
REPRESENTATION_CONTEXT('','3D')
);
#14494=(
GEOMETRIC_REPRESENTATION_CONTEXT(3)
GLOBAL_UNCERTAINTY_ASSIGNED_CONTEXT((#14437))
GLOBAL_UNIT_ASSIGNED_CONTEXT((#14513,#14515,#14516))
REPRESENTATION_CONTEXT('','3D')
);
#14495=(
GEOMETRIC_REPRESENTATION_CONTEXT(3)
GLOBAL_UNCERTAINTY_ASSIGNED_CONTEXT((#14438))
GLOBAL_UNIT_ASSIGNED_CONTEXT((#14513,#14515,#14516))
REPRESENTATION_CONTEXT('','3D')
);
#14496=(
GEOMETRIC_REPRESENTATION_CONTEXT(3)
GLOBAL_UNCERTAINTY_ASSIGNED_CONTEXT((#14439))
GLOBAL_UNIT_ASSIGNED_CONTEXT((#14513,#14515,#14516))
REPRESENTATION_CONTEXT('','3D')
);
#14497=(
GEOMETRIC_REPRESENTATION_CONTEXT(3)
GLOBAL_UNCERTAINTY_ASSIGNED_CONTEXT((#14440))
GLOBAL_UNIT_ASSIGNED_CONTEXT((#14513,#14515,#14516))
REPRESENTATION_CONTEXT('','3D')
);
#14498=(
GEOMETRIC_REPRESENTATION_CONTEXT(3)
GLOBAL_UNCERTAINTY_ASSIGNED_CONTEXT((#14441))
GLOBAL_UNIT_ASSIGNED_CONTEXT((#14513,#14515,#14516))
REPRESENTATION_CONTEXT('','3D')
);
#14499=(
GEOMETRIC_REPRESENTATION_CONTEXT(3)
GLOBAL_UNCERTAINTY_ASSIGNED_CONTEXT((#14442))
GLOBAL_UNIT_ASSIGNED_CONTEXT((#14513,#14515,#14516))
REPRESENTATION_CONTEXT('','3D')
);
#14500=(
GEOMETRIC_REPRESENTATION_CONTEXT(3)
GLOBAL_UNCERTAINTY_ASSIGNED_CONTEXT((#14443))
GLOBAL_UNIT_ASSIGNED_CONTEXT((#14513,#14515,#14516))
REPRESENTATION_CONTEXT('','3D')
);
#14501=(
GEOMETRIC_REPRESENTATION_CONTEXT(3)
GLOBAL_UNCERTAINTY_ASSIGNED_CONTEXT((#14444))
GLOBAL_UNIT_ASSIGNED_CONTEXT((#14513,#14515,#14516))
REPRESENTATION_CONTEXT('','3D')
);
#14502=(
GEOMETRIC_REPRESENTATION_CONTEXT(3)
GLOBAL_UNCERTAINTY_ASSIGNED_CONTEXT((#14445))
GLOBAL_UNIT_ASSIGNED_CONTEXT((#14513,#14515,#14516))
REPRESENTATION_CONTEXT('','3D')
);
#14503=(
GEOMETRIC_REPRESENTATION_CONTEXT(3)
GLOBAL_UNCERTAINTY_ASSIGNED_CONTEXT((#14446))
GLOBAL_UNIT_ASSIGNED_CONTEXT((#14513,#14515,#14516))
REPRESENTATION_CONTEXT('','3D')
);
#14504=(
GEOMETRIC_REPRESENTATION_CONTEXT(3)
GLOBAL_UNCERTAINTY_ASSIGNED_CONTEXT((#14447))
GLOBAL_UNIT_ASSIGNED_CONTEXT((#14513,#14515,#14516))
REPRESENTATION_CONTEXT('','3D')
);
#14505=(
GEOMETRIC_REPRESENTATION_CONTEXT(3)
GLOBAL_UNCERTAINTY_ASSIGNED_CONTEXT((#14448))
GLOBAL_UNIT_ASSIGNED_CONTEXT((#14513,#14515,#14516))
REPRESENTATION_CONTEXT('','3D')
);
#14506=(
GEOMETRIC_REPRESENTATION_CONTEXT(3)
GLOBAL_UNCERTAINTY_ASSIGNED_CONTEXT((#14449))
GLOBAL_UNIT_ASSIGNED_CONTEXT((#14513,#14515,#14516))
REPRESENTATION_CONTEXT('','3D')
);
#14507=(
GEOMETRIC_REPRESENTATION_CONTEXT(3)
GLOBAL_UNCERTAINTY_ASSIGNED_CONTEXT((#14450))
GLOBAL_UNIT_ASSIGNED_CONTEXT((#14513,#14515,#14516))
REPRESENTATION_CONTEXT('','3D')
);
#14508=(
GEOMETRIC_REPRESENTATION_CONTEXT(3)
GLOBAL_UNCERTAINTY_ASSIGNED_CONTEXT((#14451))
GLOBAL_UNIT_ASSIGNED_CONTEXT((#14513,#14515,#14516))
REPRESENTATION_CONTEXT('','3D')
);
#14509=(
GEOMETRIC_REPRESENTATION_CONTEXT(3)
GLOBAL_UNCERTAINTY_ASSIGNED_CONTEXT((#14452))
GLOBAL_UNIT_ASSIGNED_CONTEXT((#14513,#14515,#14516))
REPRESENTATION_CONTEXT('','3D')
);
#14510=(
GEOMETRIC_REPRESENTATION_CONTEXT(3)
GLOBAL_UNCERTAINTY_ASSIGNED_CONTEXT((#14453))
GLOBAL_UNIT_ASSIGNED_CONTEXT((#14513,#14515,#14516))
REPRESENTATION_CONTEXT('','3D')
);
#14511=(
GEOMETRIC_REPRESENTATION_CONTEXT(3)
GLOBAL_UNCERTAINTY_ASSIGNED_CONTEXT((#14454))
GLOBAL_UNIT_ASSIGNED_CONTEXT((#14513,#14515,#14516))
REPRESENTATION_CONTEXT('','3D')
);
#14512=(
GEOMETRIC_REPRESENTATION_CONTEXT(3)
GLOBAL_UNCERTAINTY_ASSIGNED_CONTEXT((#14455))
GLOBAL_UNIT_ASSIGNED_CONTEXT((#14513,#14515,#14516))
REPRESENTATION_CONTEXT('','3D')
);
#14513=(
LENGTH_UNIT()
NAMED_UNIT(*)
SI_UNIT(.CENTI.,.METRE.)
);
#14514=(
LENGTH_UNIT()
NAMED_UNIT(*)
SI_UNIT($,.METRE.)
);
#14515=(
NAMED_UNIT(*)
PLANE_ANGLE_UNIT()
SI_UNIT($,.RADIAN.)
);
#14516=(
NAMED_UNIT(*)
SI_UNIT($,.STERADIAN.)
SOLID_ANGLE_UNIT()
);
#14517=SHAPE_DEFINITION_REPRESENTATION(#14573,#14741);
#14518=SHAPE_DEFINITION_REPRESENTATION(#14574,#14742);
#14519=SHAPE_DEFINITION_REPRESENTATION(#14575,#14743);
#14520=SHAPE_DEFINITION_REPRESENTATION(#14576,#14744);
#14521=SHAPE_DEFINITION_REPRESENTATION(#14577,#14745);
#14522=SHAPE_DEFINITION_REPRESENTATION(#14578,#14746);
#14523=SHAPE_DEFINITION_REPRESENTATION(#14579,#14747);
#14524=SHAPE_DEFINITION_REPRESENTATION(#14580,#14748);
#14525=SHAPE_DEFINITION_REPRESENTATION(#14581,#14749);
#14526=SHAPE_DEFINITION_REPRESENTATION(#14582,#14750);
#14527=SHAPE_DEFINITION_REPRESENTATION(#14583,#14751);
#14528=SHAPE_DEFINITION_REPRESENTATION(#14584,#14752);
#14529=SHAPE_DEFINITION_REPRESENTATION(#14585,#14753);
#14530=SHAPE_DEFINITION_REPRESENTATION(#14586,#14754);
#14531=SHAPE_DEFINITION_REPRESENTATION(#14587,#14755);
#14532=SHAPE_DEFINITION_REPRESENTATION(#14588,#14756);
#14533=SHAPE_DEFINITION_REPRESENTATION(#14589,#14757);
#14534=SHAPE_DEFINITION_REPRESENTATION(#14590,#14758);
#14535=SHAPE_DEFINITION_REPRESENTATION(#14591,#14759);
#14536=SHAPE_DEFINITION_REPRESENTATION(#14592,#14760);
#14537=SHAPE_DEFINITION_REPRESENTATION(#14593,#14761);
#14538=SHAPE_DEFINITION_REPRESENTATION(#14594,#14762);
#14539=SHAPE_DEFINITION_REPRESENTATION(#14595,#14763);
#14540=SHAPE_DEFINITION_REPRESENTATION(#14596,#14764);
#14541=SHAPE_DEFINITION_REPRESENTATION(#14597,#14765);
#14542=SHAPE_DEFINITION_REPRESENTATION(#14598,#14766);
#14543=SHAPE_DEFINITION_REPRESENTATION(#14599,#14767);
#14544=SHAPE_DEFINITION_REPRESENTATION(#14600,#14768);
#14545=SHAPE_DEFINITION_REPRESENTATION(#14601,#14769);
#14546=SHAPE_DEFINITION_REPRESENTATION(#14602,#14770);
#14547=SHAPE_DEFINITION_REPRESENTATION(#14603,#14771);
#14548=SHAPE_DEFINITION_REPRESENTATION(#14604,#14772);
#14549=SHAPE_DEFINITION_REPRESENTATION(#14605,#14773);
#14550=SHAPE_DEFINITION_REPRESENTATION(#14606,#14774);
#14551=SHAPE_DEFINITION_REPRESENTATION(#14607,#14775);
#14552=SHAPE_DEFINITION_REPRESENTATION(#14608,#14776);
#14553=SHAPE_DEFINITION_REPRESENTATION(#14609,#14777);
#14554=SHAPE_DEFINITION_REPRESENTATION(#14610,#14778);
#14555=SHAPE_DEFINITION_REPRESENTATION(#14611,#14779);
#14556=SHAPE_DEFINITION_REPRESENTATION(#14612,#14780);
#14557=SHAPE_DEFINITION_REPRESENTATION(#14613,#14781);
#14558=SHAPE_DEFINITION_REPRESENTATION(#14614,#14782);
#14559=SHAPE_DEFINITION_REPRESENTATION(#14620,#14783);
#14560=SHAPE_DEFINITION_REPRESENTATION(#14676,#14784);
#14561=SHAPE_DEFINITION_REPRESENTATION(#14677,#14785);
#14562=SHAPE_DEFINITION_REPRESENTATION(#14678,#14786);
#14563=SHAPE_DEFINITION_REPRESENTATION(#14679,#14787);
#14564=SHAPE_DEFINITION_REPRESENTATION(#14680,#14788);
#14565=SHAPE_DEFINITION_REPRESENTATION(#14681,#14789);
#14566=SHAPE_DEFINITION_REPRESENTATION(#14682,#14790);
#14567=SHAPE_DEFINITION_REPRESENTATION(#14683,#14791);
#14568=SHAPE_DEFINITION_REPRESENTATION(#14684,#14792);
#14569=SHAPE_DEFINITION_REPRESENTATION(#14685,#14793);
#14570=SHAPE_DEFINITION_REPRESENTATION(#14686,#14794);
#14571=SHAPE_DEFINITION_REPRESENTATION(#14687,#14795);
#14572=SHAPE_DEFINITION_REPRESENTATION(#14688,#14796);
#14573=PRODUCT_DEFINITION_SHAPE('',$,#14798);
#14574=PRODUCT_DEFINITION_SHAPE('',$,#14799);
#14575=PRODUCT_DEFINITION_SHAPE('',$,#14800);
#14576=PRODUCT_DEFINITION_SHAPE('',$,#14801);
#14577=PRODUCT_DEFINITION_SHAPE('',$,#14802);
#14578=PRODUCT_DEFINITION_SHAPE('',$,#14803);
#14579=PRODUCT_DEFINITION_SHAPE('',$,#14804);
#14580=PRODUCT_DEFINITION_SHAPE('',$,#14805);
#14581=PRODUCT_DEFINITION_SHAPE('',$,#14806);
#14582=PRODUCT_DEFINITION_SHAPE('',$,#14807);
#14583=PRODUCT_DEFINITION_SHAPE('',$,#14808);
#14584=PRODUCT_DEFINITION_SHAPE('',$,#14809);
#14585=PRODUCT_DEFINITION_SHAPE('',$,#14810);
#14586=PRODUCT_DEFINITION_SHAPE('',$,#14811);
#14587=PRODUCT_DEFINITION_SHAPE('',$,#14812);
#14588=PRODUCT_DEFINITION_SHAPE('',$,#14813);
#14589=PRODUCT_DEFINITION_SHAPE('',$,#14814);
#14590=PRODUCT_DEFINITION_SHAPE('',$,#14815);
#14591=PRODUCT_DEFINITION_SHAPE('',$,#14816);
#14592=PRODUCT_DEFINITION_SHAPE('',$,#14817);
#14593=PRODUCT_DEFINITION_SHAPE('',$,#14818);
#14594=PRODUCT_DEFINITION_SHAPE('',$,#14819);
#14595=PRODUCT_DEFINITION_SHAPE('',$,#14820);
#14596=PRODUCT_DEFINITION_SHAPE('',$,#14821);
#14597=PRODUCT_DEFINITION_SHAPE('',$,#14822);
#14598=PRODUCT_DEFINITION_SHAPE('',$,#14823);
#14599=PRODUCT_DEFINITION_SHAPE('',$,#14824);
#14600=PRODUCT_DEFINITION_SHAPE('',$,#14825);
#14601=PRODUCT_DEFINITION_SHAPE('',$,#14826);
#14602=PRODUCT_DEFINITION_SHAPE('',$,#14827);
#14603=PRODUCT_DEFINITION_SHAPE('',$,#14828);
#14604=PRODUCT_DEFINITION_SHAPE('',$,#14829);
#14605=PRODUCT_DEFINITION_SHAPE('',$,#14830);
#14606=PRODUCT_DEFINITION_SHAPE('',$,#14831);
#14607=PRODUCT_DEFINITION_SHAPE('',$,#14832);
#14608=PRODUCT_DEFINITION_SHAPE('',$,#14833);
#14609=PRODUCT_DEFINITION_SHAPE('',$,#14834);
#14610=PRODUCT_DEFINITION_SHAPE('',$,#14835);
#14611=PRODUCT_DEFINITION_SHAPE('',$,#14836);
#14612=PRODUCT_DEFINITION_SHAPE('',$,#14837);
#14613=PRODUCT_DEFINITION_SHAPE('',$,#14838);
#14614=PRODUCT_DEFINITION_SHAPE('',$,#14839);
#14615=PRODUCT_DEFINITION_SHAPE($,$,#347);
#14616=PRODUCT_DEFINITION_SHAPE($,$,#348);
#14617=PRODUCT_DEFINITION_SHAPE($,$,#349);
#14618=PRODUCT_DEFINITION_SHAPE($,$,#350);
#14619=PRODUCT_DEFINITION_SHAPE($,$,#351);
#14620=PRODUCT_DEFINITION_SHAPE('',$,#14840);
#14621=PRODUCT_DEFINITION_SHAPE($,$,#352);
#14622=PRODUCT_DEFINITION_SHAPE($,$,#353);
#14623=PRODUCT_DEFINITION_SHAPE($,$,#354);
#14624=PRODUCT_DEFINITION_SHAPE($,$,#355);
#14625=PRODUCT_DEFINITION_SHAPE($,$,#356);
#14626=PRODUCT_DEFINITION_SHAPE($,$,#357);
#14627=PRODUCT_DEFINITION_SHAPE($,$,#358);
#14628=PRODUCT_DEFINITION_SHAPE($,$,#359);
#14629=PRODUCT_DEFINITION_SHAPE($,$,#360);
#14630=PRODUCT_DEFINITION_SHAPE($,$,#361);
#14631=PRODUCT_DEFINITION_SHAPE($,$,#362);
#14632=PRODUCT_DEFINITION_SHAPE($,$,#363);
#14633=PRODUCT_DEFINITION_SHAPE($,$,#364);
#14634=PRODUCT_DEFINITION_SHAPE($,$,#365);
#14635=PRODUCT_DEFINITION_SHAPE($,$,#366);
#14636=PRODUCT_DEFINITION_SHAPE($,$,#367);
#14637=PRODUCT_DEFINITION_SHAPE($,$,#368);
#14638=PRODUCT_DEFINITION_SHAPE($,$,#369);
#14639=PRODUCT_DEFINITION_SHAPE($,$,#370);
#14640=PRODUCT_DEFINITION_SHAPE($,$,#371);
#14641=PRODUCT_DEFINITION_SHAPE($,$,#372);
#14642=PRODUCT_DEFINITION_SHAPE($,$,#373);
#14643=PRODUCT_DEFINITION_SHAPE($,$,#374);
#14644=PRODUCT_DEFINITION_SHAPE($,$,#375);
#14645=PRODUCT_DEFINITION_SHAPE($,$,#376);
#14646=PRODUCT_DEFINITION_SHAPE($,$,#377);
#14647=PRODUCT_DEFINITION_SHAPE($,$,#378);
#14648=PRODUCT_DEFINITION_SHAPE($,$,#379);
#14649=PRODUCT_DEFINITION_SHAPE($,$,#380);
#14650=PRODUCT_DEFINITION_SHAPE($,$,#381);
#14651=PRODUCT_DEFINITION_SHAPE($,$,#382);
#14652=PRODUCT_DEFINITION_SHAPE($,$,#383);
#14653=PRODUCT_DEFINITION_SHAPE($,$,#384);
#14654=PRODUCT_DEFINITION_SHAPE($,$,#385);
#14655=PRODUCT_DEFINITION_SHAPE($,$,#386);
#14656=PRODUCT_DEFINITION_SHAPE($,$,#387);
#14657=PRODUCT_DEFINITION_SHAPE($,$,#388);
#14658=PRODUCT_DEFINITION_SHAPE($,$,#389);
#14659=PRODUCT_DEFINITION_SHAPE($,$,#390);
#14660=PRODUCT_DEFINITION_SHAPE($,$,#391);
#14661=PRODUCT_DEFINITION_SHAPE($,$,#392);
#14662=PRODUCT_DEFINITION_SHAPE($,$,#393);
#14663=PRODUCT_DEFINITION_SHAPE($,$,#394);
#14664=PRODUCT_DEFINITION_SHAPE($,$,#395);
#14665=PRODUCT_DEFINITION_SHAPE($,$,#396);
#14666=PRODUCT_DEFINITION_SHAPE($,$,#397);
#14667=PRODUCT_DEFINITION_SHAPE($,$,#398);
#14668=PRODUCT_DEFINITION_SHAPE($,$,#399);
#14669=PRODUCT_DEFINITION_SHAPE($,$,#400);
#14670=PRODUCT_DEFINITION_SHAPE($,$,#401);
#14671=PRODUCT_DEFINITION_SHAPE($,$,#402);
#14672=PRODUCT_DEFINITION_SHAPE($,$,#403);
#14673=PRODUCT_DEFINITION_SHAPE($,$,#404);
#14674=PRODUCT_DEFINITION_SHAPE($,$,#405);
#14675=PRODUCT_DEFINITION_SHAPE($,$,#406);
#14676=PRODUCT_DEFINITION_SHAPE('',$,#14841);
#14677=PRODUCT_DEFINITION_SHAPE('',$,#14842);
#14678=PRODUCT_DEFINITION_SHAPE('',$,#14843);
#14679=PRODUCT_DEFINITION_SHAPE('',$,#14844);
#14680=PRODUCT_DEFINITION_SHAPE('',$,#14845);
#14681=PRODUCT_DEFINITION_SHAPE('',$,#14846);
#14682=PRODUCT_DEFINITION_SHAPE('',$,#14847);
#14683=PRODUCT_DEFINITION_SHAPE('',$,#14848);
#14684=PRODUCT_DEFINITION_SHAPE('',$,#14849);
#14685=PRODUCT_DEFINITION_SHAPE('',$,#14850);
#14686=PRODUCT_DEFINITION_SHAPE('',$,#14851);
#14687=PRODUCT_DEFINITION_SHAPE('',$,#14852);
#14688=PRODUCT_DEFINITION_SHAPE('',$,#14853);
#14689=PRODUCT_DEFINITION_SHAPE($,$,#407);
#14690=PRODUCT_DEFINITION_SHAPE($,$,#408);
#14691=PRODUCT_DEFINITION_SHAPE($,$,#409);
#14692=PRODUCT_DEFINITION_SHAPE($,$,#410);
#14693=PRODUCT_DEFINITION_SHAPE($,$,#411);
#14694=PRODUCT_DEFINITION_SHAPE($,$,#412);
#14695=PRODUCT_DEFINITION_SHAPE($,$,#413);
#14696=PRODUCT_DEFINITION_SHAPE($,$,#414);
#14697=PRODUCT_DEFINITION_SHAPE($,$,#415);
#14698=PRODUCT_DEFINITION_SHAPE($,$,#416);
#14699=PRODUCT_DEFINITION_SHAPE($,$,#417);
#14700=PRODUCT_DEFINITION_SHAPE($,$,#418);
#14701=PRODUCT_DEFINITION_SHAPE($,$,#419);
#14702=PRODUCT_DEFINITION_SHAPE($,$,#420);
#14703=PRODUCT_DEFINITION_SHAPE($,$,#421);
#14704=PRODUCT_DEFINITION_SHAPE($,$,#422);
#14705=PRODUCT_DEFINITION_SHAPE($,$,#423);
#14706=PRODUCT_DEFINITION_SHAPE($,$,#424);
#14707=PRODUCT_DEFINITION_SHAPE($,$,#425);
#14708=PRODUCT_DEFINITION_SHAPE($,$,#426);
#14709=PRODUCT_DEFINITION_SHAPE($,$,#427);
#14710=PRODUCT_DEFINITION_SHAPE($,$,#428);
#14711=PRODUCT_DEFINITION_SHAPE($,$,#429);
#14712=PRODUCT_DEFINITION_SHAPE($,$,#430);
#14713=PRODUCT_DEFINITION_SHAPE($,$,#431);
#14714=PRODUCT_DEFINITION_SHAPE($,$,#432);
#14715=PRODUCT_DEFINITION_SHAPE($,$,#433);
#14716=PRODUCT_DEFINITION_SHAPE($,$,#434);
#14717=PRODUCT_DEFINITION_SHAPE($,$,#435);
#14718=PRODUCT_DEFINITION_SHAPE($,$,#436);
#14719=PRODUCT_DEFINITION_SHAPE($,$,#437);
#14720=PRODUCT_DEFINITION_SHAPE($,$,#438);
#14721=PRODUCT_DEFINITION_SHAPE($,$,#439);
#14722=PRODUCT_DEFINITION_SHAPE($,$,#440);
#14723=PRODUCT_DEFINITION_SHAPE($,$,#441);
#14724=PRODUCT_DEFINITION_SHAPE($,$,#442);
#14725=PRODUCT_DEFINITION_SHAPE($,$,#443);
#14726=PRODUCT_DEFINITION_SHAPE($,$,#444);
#14727=PRODUCT_DEFINITION_SHAPE($,$,#445);
#14728=PRODUCT_DEFINITION_SHAPE($,$,#446);
#14729=PRODUCT_DEFINITION_SHAPE($,$,#447);
#14730=PRODUCT_DEFINITION_SHAPE($,$,#448);
#14731=PRODUCT_DEFINITION_SHAPE($,$,#449);
#14732=PRODUCT_DEFINITION_SHAPE($,$,#450);
#14733=PRODUCT_DEFINITION_SHAPE($,$,#451);
#14734=PRODUCT_DEFINITION_SHAPE($,$,#452);
#14735=PRODUCT_DEFINITION_SHAPE($,$,#453);
#14736=PRODUCT_DEFINITION_SHAPE($,$,#454);
#14737=PRODUCT_DEFINITION_SHAPE($,$,#455);
#14738=PRODUCT_DEFINITION_SHAPE($,$,#456);
#14739=PRODUCT_DEFINITION_SHAPE($,$,#457);
#14740=PRODUCT_DEFINITION_SHAPE($,$,#458);
#14741=SHAPE_REPRESENTATION('',(#7938,#8966,#8967,#8968,#8969),#14456);
#14742=SHAPE_REPRESENTATION('',(#7939,#8918,#8919,#8920,#8921,#8922,#8923,
#8924,#8925,#8926,#8927,#8928,#8929,#8930,#8931,#8932,#8933,#8934,#8935,
#8936,#8937,#8938,#8939,#8940,#8941,#8942,#8943,#8944,#8945,#8946),#14457);
#14743=SHAPE_REPRESENTATION('',(#7940),#14458);
#14744=SHAPE_REPRESENTATION('',(#7959),#14459);
#14745=SHAPE_REPRESENTATION('',(#7966),#14460);
#14746=SHAPE_REPRESENTATION('',(#7973),#14461);
#14747=SHAPE_REPRESENTATION('',(#8024),#14462);
#14748=SHAPE_REPRESENTATION('',(#8051),#14463);
#14749=SHAPE_REPRESENTATION('',(#8060),#14464);
#14750=SHAPE_REPRESENTATION('',(#8069),#14465);
#14751=SHAPE_REPRESENTATION('',(#8078),#14466);
#14752=SHAPE_REPRESENTATION('',(#8087),#14467);
#14753=SHAPE_REPRESENTATION('',(#8114),#14468);
#14754=SHAPE_REPRESENTATION('',(#8123),#14469);
#14755=SHAPE_REPRESENTATION('',(#8132),#14470);
#14756=SHAPE_REPRESENTATION('',(#8141),#14471);
#14757=SHAPE_REPRESENTATION('',(#8150),#14472);
#14758=SHAPE_REPRESENTATION('',(#8168),#14473);
#14759=SHAPE_REPRESENTATION('',(#8184),#14474);
#14760=SHAPE_REPRESENTATION('',(#8208,#8664,#8665,#8666,#8667,#8668,#8669,
#8670,#8671,#8672,#8673,#8674,#8675,#8676,#8677,#8678,#8679,#8680,#8681,
#8682,#8683,#8684,#8685,#8686,#8687,#8688,#8689,#8690,#8691),#14475);
#14761=SHAPE_REPRESENTATION('',(#8209),#14476);
#14762=SHAPE_REPRESENTATION('',(#8250),#14477);
#14763=SHAPE_REPRESENTATION('',(#8259),#14478);
#14764=SHAPE_REPRESENTATION('',(#8280),#14479);
#14765=SHAPE_REPRESENTATION('',(#8301),#14480);
#14766=SHAPE_REPRESENTATION('',(#8310),#14481);
#14767=SHAPE_REPRESENTATION('',(#8331),#14482);
#14768=SHAPE_REPRESENTATION('',(#8352),#14483);
#14769=SHAPE_REPRESENTATION('',(#8362,#8692,#8693,#8694,#8695,#8696,#8697,
#8698,#8699,#8700,#8701,#8702,#8703,#8704,#8705,#8706,#8707,#8708,#8709,
#8710,#8711,#8712,#8713,#8714,#8715,#8716,#8717,#8718),#14484);
#14770=SHAPE_REPRESENTATION('',(#8363),#14485);
#14771=SHAPE_REPRESENTATION('',(#8404),#14486);
#14772=SHAPE_REPRESENTATION('',(#8413),#14487);
#14773=SHAPE_REPRESENTATION('',(#8434),#14488);
#14774=SHAPE_REPRESENTATION('',(#8455),#14489);
#14775=SHAPE_REPRESENTATION('',(#8464),#14490);
#14776=SHAPE_REPRESENTATION('',(#8485),#14491);
#14777=SHAPE_REPRESENTATION('',(#8506,#8635,#8636,#8637,#8638,#8639),#14492);
#14778=SHAPE_REPRESENTATION('',(#8507),#14493);
#14779=SHAPE_REPRESENTATION('',(#8527),#14494);
#14780=SHAPE_REPRESENTATION('',(#8547),#14495);
#14781=SHAPE_REPRESENTATION('',(#8564),#14496);
#14782=SHAPE_REPRESENTATION('',(#8618),#14497);
#14783=SHAPE_REPRESENTATION('',(#8640),#14498);
#14784=SHAPE_REPRESENTATION('',(#8719,#8947,#8948,#8949,#8950,#8951,#8952,
#8953,#8954,#8955,#8956,#8957,#8958,#8959,#8960,#8961,#8962,#8963,#8964,
#8965),#14499);
#14785=SHAPE_REPRESENTATION('',(#8720),#14500);
#14786=SHAPE_REPRESENTATION('',(#8766),#14501);
#14787=SHAPE_REPRESENTATION('',(#8793),#14502);
#14788=SHAPE_REPRESENTATION('',(#8802),#14503);
#14789=SHAPE_REPRESENTATION('',(#8811),#14504);
#14790=SHAPE_REPRESENTATION('',(#8820),#14505);
#14791=SHAPE_REPRESENTATION('',(#8829),#14506);
#14792=SHAPE_REPRESENTATION('',(#8856),#14507);
#14793=SHAPE_REPRESENTATION('',(#8865),#14508);
#14794=SHAPE_REPRESENTATION('',(#8874),#14509);
#14795=SHAPE_REPRESENTATION('',(#8883),#14510);
#14796=SHAPE_REPRESENTATION('',(#8892),#14511);
#14797=PRODUCT_DEFINITION_CONTEXT('part definition',#14967,'design');
#14798=PRODUCT_DEFINITION('PAT-039','PAT-039',#14854,
#14797);
#14799=PRODUCT_DEFINITION('Fixed bracket and counter spring',
'Fixed bracket and counter spring',#14855,#14797);
#14800=PRODUCT_DEFINITION('Base','Base',#14856,#14797);
#14801=PRODUCT_DEFINITION('Foot strip','Foot strip',#14857,#14797);
#14802=PRODUCT_DEFINITION('Foot strip (1)','Foot strip (1)',#14858,#14797);
#14803=PRODUCT_DEFINITION('Fixed link','Fixed link',#14859,#14797);
#14804=PRODUCT_DEFINITION('Spring arbor pivot','Spring arbor pivot',#14860,
#14797);
#14805=PRODUCT_DEFINITION('Inner race sleeve','Inner race sleeve',#14861,
#14797);
#14806=PRODUCT_DEFINITION('Rear inner spacer','Rear inner spacer',#14862,
#14797);
#14807=PRODUCT_DEFINITION('Long front spacer','Long front spacer',#14863,
#14797);
#14808=PRODUCT_DEFINITION('Pivot keeper','Pivot keeper',#14864,#14797);
#14809=PRODUCT_DEFINITION('Pivot pin','Pivot pin',#14865,#14797);
#14810=PRODUCT_DEFINITION('Inner race sleeve (1)','Inner race sleeve (1)',
#14866,#14797);
#14811=PRODUCT_DEFINITION('Rear inner spacer (1)','Rear inner spacer (1)',
#14867,#14797);
#14812=PRODUCT_DEFINITION('Front spacer','Front spacer',#14868,#14797);
#14813=PRODUCT_DEFINITION('Pivot keeper (1)','Pivot keeper (1)',#14869,#14797);
#14814=PRODUCT_DEFINITION('Fixed spring bracket','Fixed spring bracket',
#14870,#14797);
#14815=PRODUCT_DEFINITION('Installed torsion spring',
'Installed torsion spring',#14871,#14797);
#14816=PRODUCT_DEFINITION('M5x14 Cap Screw','M5x14 Cap Screw',#14872,#14797);
#14817=PRODUCT_DEFINITION('Lower link','Lower link',#14873,#14797);
#14818=PRODUCT_DEFINITION('200 mm arm','200 mm arm',#14874,#14797);
#14819=PRODUCT_DEFINITION('Outer race spacer','Outer race spacer',#14875,
#14797);
#14820=PRODUCT_DEFINITION('Bearing cap','Bearing cap',#14876,#14797);
#14821=PRODUCT_DEFINITION('Bearing cap (1)','Bearing cap (1)',#14877,#14797);
#14822=PRODUCT_DEFINITION('Outer race spacer (1)','Outer race spacer (1)',
#14878,#14797);
#14823=PRODUCT_DEFINITION('Bearing cap (2)','Bearing cap (2)',#14879,#14797);
#14824=PRODUCT_DEFINITION('Bearing cap (3)','Bearing cap (3)',#14880,#14797);
#14825=PRODUCT_DEFINITION('Moving spring anchor','Moving spring anchor',
#14881,#14797);
#14826=PRODUCT_DEFINITION('Upper link','Upper link',#14882,#14797);
#14827=PRODUCT_DEFINITION('200 mm arm (1)','200 mm arm (1)',#14883,#14797);
#14828=PRODUCT_DEFINITION('Outer race spacer (2)','Outer race spacer (2)',
#14884,#14797);
#14829=PRODUCT_DEFINITION('Bearing cap (4)','Bearing cap (4)',#14885,#14797);
#14830=PRODUCT_DEFINITION('Bearing cap (5)','Bearing cap (5)',#14886,#14797);
#14831=PRODUCT_DEFINITION('Outer race spacer (3)','Outer race spacer (3)',
#14887,#14797);
#14832=PRODUCT_DEFINITION('Bearing cap (6)','Bearing cap (6)',#14888,#14797);
#14833=PRODUCT_DEFINITION('Bearing cap (7)','Bearing cap (7)',#14889,#14797);
#14834=PRODUCT_DEFINITION('Sealed Ball Bearing - 10 x 30 x 9 mm',
'Sealed Ball Bearing - 10 x 30 x 9 mm',#14890,#14797);
#14835=PRODUCT_DEFINITION('Inner ring','Inner ring',#14891,#14797);
#14836=PRODUCT_DEFINITION('Outer ring','Outer ring',#14892,#14797);
#14837=PRODUCT_DEFINITION('Balls','Balls',#14893,#14797);
#14838=PRODUCT_DEFINITION('Cage','Cage',#14894,#14797);
#14839=PRODUCT_DEFINITION('Seals 2RS','Seals 2RS',#14895,#14797);
#14840=PRODUCT_DEFINITION('M4x10 Cap Screw','M4x10 Cap Screw',#14896,#14797);
#14841=PRODUCT_DEFINITION('Level platform link','Level platform link',#14897,
#14797);
#14842=PRODUCT_DEFINITION('Platform link','Platform link',#14898,#14797);
#14843=PRODUCT_DEFINITION('Pivot pin (1)','Pivot pin (1)',#14899,#14797);
#14844=PRODUCT_DEFINITION('Inner race sleeve (2)','Inner race sleeve (2)',
#14900,#14797);
#14845=PRODUCT_DEFINITION('Rear inner spacer (2)','Rear inner spacer (2)',
#14901,#14797);
#14846=PRODUCT_DEFINITION('Front spacer (1)','Front spacer (1)',#14902,#14797);
#14847=PRODUCT_DEFINITION('Pivot keeper (2)','Pivot keeper (2)',#14903,#14797);
#14848=PRODUCT_DEFINITION('Pivot pin (2)','Pivot pin (2)',#14904,#14797);
#14849=PRODUCT_DEFINITION('Inner race sleeve (3)','Inner race sleeve (3)',
#14905,#14797);
#14850=PRODUCT_DEFINITION('Rear inner spacer (3)','Rear inner spacer (3)',
#14906,#14797);
#14851=PRODUCT_DEFINITION('Front spacer (2)','Front spacer (2)',#14907,#14797);
#14852=PRODUCT_DEFINITION('Pivot keeper (3)','Pivot keeper (3)',#14908,#14797);
#14853=PRODUCT_DEFINITION('Cap Screw - M4x16','Cap Screw - M4x16',#14909,
#14797);
#14854=PRODUCT_DEFINITION_FORMATION('',$,#14969);
#14855=PRODUCT_DEFINITION_FORMATION('',$,#14970);
#14856=PRODUCT_DEFINITION_FORMATION('',$,#14971);
#14857=PRODUCT_DEFINITION_FORMATION('',$,#14972);
#14858=PRODUCT_DEFINITION_FORMATION('',$,#14973);
#14859=PRODUCT_DEFINITION_FORMATION('',$,#14974);
#14860=PRODUCT_DEFINITION_FORMATION('',$,#14975);
#14861=PRODUCT_DEFINITION_FORMATION('',$,#14976);
#14862=PRODUCT_DEFINITION_FORMATION('',$,#14977);
#14863=PRODUCT_DEFINITION_FORMATION('',$,#14978);
#14864=PRODUCT_DEFINITION_FORMATION('',$,#14979);
#14865=PRODUCT_DEFINITION_FORMATION('',$,#14980);
#14866=PRODUCT_DEFINITION_FORMATION('',$,#14981);
#14867=PRODUCT_DEFINITION_FORMATION('',$,#14982);
#14868=PRODUCT_DEFINITION_FORMATION('',$,#14983);
#14869=PRODUCT_DEFINITION_FORMATION('',$,#14984);
#14870=PRODUCT_DEFINITION_FORMATION('',$,#14985);
#14871=PRODUCT_DEFINITION_FORMATION('',$,#14986);
#14872=PRODUCT_DEFINITION_FORMATION('',$,#14987);
#14873=PRODUCT_DEFINITION_FORMATION('',$,#14988);
#14874=PRODUCT_DEFINITION_FORMATION('',$,#14989);
#14875=PRODUCT_DEFINITION_FORMATION('',$,#14990);
#14876=PRODUCT_DEFINITION_FORMATION('',$,#14991);
#14877=PRODUCT_DEFINITION_FORMATION('',$,#14992);
#14878=PRODUCT_DEFINITION_FORMATION('',$,#14993);
#14879=PRODUCT_DEFINITION_FORMATION('',$,#14994);
#14880=PRODUCT_DEFINITION_FORMATION('',$,#14995);
#14881=PRODUCT_DEFINITION_FORMATION('',$,#14996);
#14882=PRODUCT_DEFINITION_FORMATION('',$,#14997);
#14883=PRODUCT_DEFINITION_FORMATION('',$,#14998);
#14884=PRODUCT_DEFINITION_FORMATION('',$,#14999);
#14885=PRODUCT_DEFINITION_FORMATION('',$,#15000);
#14886=PRODUCT_DEFINITION_FORMATION('',$,#15001);
#14887=PRODUCT_DEFINITION_FORMATION('',$,#15002);
#14888=PRODUCT_DEFINITION_FORMATION('',$,#15003);
#14889=PRODUCT_DEFINITION_FORMATION('',$,#15004);
#14890=PRODUCT_DEFINITION_FORMATION('',$,#15005);
#14891=PRODUCT_DEFINITION_FORMATION('',$,#15006);
#14892=PRODUCT_DEFINITION_FORMATION('',$,#15007);
#14893=PRODUCT_DEFINITION_FORMATION('',$,#15008);
#14894=PRODUCT_DEFINITION_FORMATION('',$,#15009);
#14895=PRODUCT_DEFINITION_FORMATION('',$,#15010);
#14896=PRODUCT_DEFINITION_FORMATION('',$,#15011);
#14897=PRODUCT_DEFINITION_FORMATION('',$,#15012);
#14898=PRODUCT_DEFINITION_FORMATION('',$,#15013);
#14899=PRODUCT_DEFINITION_FORMATION('',$,#15014);
#14900=PRODUCT_DEFINITION_FORMATION('',$,#15015);
#14901=PRODUCT_DEFINITION_FORMATION('',$,#15016);
#14902=PRODUCT_DEFINITION_FORMATION('',$,#15017);
#14903=PRODUCT_DEFINITION_FORMATION('',$,#15018);
#14904=PRODUCT_DEFINITION_FORMATION('',$,#15019);
#14905=PRODUCT_DEFINITION_FORMATION('',$,#15020);
#14906=PRODUCT_DEFINITION_FORMATION('',$,#15021);
#14907=PRODUCT_DEFINITION_FORMATION('',$,#15022);
#14908=PRODUCT_DEFINITION_FORMATION('',$,#15023);
#14909=PRODUCT_DEFINITION_FORMATION('',$,#15024);
#14910=PRODUCT_RELATED_PRODUCT_CATEGORY('PAT-039','PAT-039',(#14969));
#14911=PRODUCT_RELATED_PRODUCT_CATEGORY(
'Fixed bracket and counter spring','Fixed bracket and counter spring',(#14970));
#14912=PRODUCT_RELATED_PRODUCT_CATEGORY('Base','Base',(#14971));
#14913=PRODUCT_RELATED_PRODUCT_CATEGORY('Foot strip','Foot strip',(#14972));
#14914=PRODUCT_RELATED_PRODUCT_CATEGORY('Foot strip (1)',
'Foot strip (1)',(#14973));
#14915=PRODUCT_RELATED_PRODUCT_CATEGORY('Fixed link','Fixed link',(#14974));
#14916=PRODUCT_RELATED_PRODUCT_CATEGORY('Spring arbor pivot',
'Spring arbor pivot',(#14975));
#14917=PRODUCT_RELATED_PRODUCT_CATEGORY('Inner race sleeve',
'Inner race sleeve',(#14976));
#14918=PRODUCT_RELATED_PRODUCT_CATEGORY('Rear inner spacer',
'Rear inner spacer',(#14977));
#14919=PRODUCT_RELATED_PRODUCT_CATEGORY('Long front spacer',
'Long front spacer',(#14978));
#14920=PRODUCT_RELATED_PRODUCT_CATEGORY('Pivot keeper','Pivot keeper',(#14979));
#14921=PRODUCT_RELATED_PRODUCT_CATEGORY('Pivot pin','Pivot pin',(#14980));
#14922=PRODUCT_RELATED_PRODUCT_CATEGORY('Inner race sleeve (1)',
'Inner race sleeve (1)',(#14981));
#14923=PRODUCT_RELATED_PRODUCT_CATEGORY('Rear inner spacer (1)',
'Rear inner spacer (1)',(#14982));
#14924=PRODUCT_RELATED_PRODUCT_CATEGORY('Front spacer','Front spacer',(#14983));
#14925=PRODUCT_RELATED_PRODUCT_CATEGORY('Pivot keeper (1)',
'Pivot keeper (1)',(#14984));
#14926=PRODUCT_RELATED_PRODUCT_CATEGORY('Fixed spring bracket',
'Fixed spring bracket',(#14985));
#14927=PRODUCT_RELATED_PRODUCT_CATEGORY('Installed torsion spring',
'Installed torsion spring',(#14986));
#14928=PRODUCT_RELATED_PRODUCT_CATEGORY('M5x14 Cap Screw',
'M5x14 Cap Screw',(#14987));
#14929=PRODUCT_RELATED_PRODUCT_CATEGORY('Lower link','Lower link',(#14988));
#14930=PRODUCT_RELATED_PRODUCT_CATEGORY('200 mm arm','200 mm arm',(#14989));
#14931=PRODUCT_RELATED_PRODUCT_CATEGORY('Outer race spacer',
'Outer race spacer',(#14990));
#14932=PRODUCT_RELATED_PRODUCT_CATEGORY('Bearing cap','Bearing cap',(#14991));
#14933=PRODUCT_RELATED_PRODUCT_CATEGORY('Bearing cap (1)',
'Bearing cap (1)',(#14992));
#14934=PRODUCT_RELATED_PRODUCT_CATEGORY('Outer race spacer (1)',
'Outer race spacer (1)',(#14993));
#14935=PRODUCT_RELATED_PRODUCT_CATEGORY('Bearing cap (2)',
'Bearing cap (2)',(#14994));
#14936=PRODUCT_RELATED_PRODUCT_CATEGORY('Bearing cap (3)',
'Bearing cap (3)',(#14995));
#14937=PRODUCT_RELATED_PRODUCT_CATEGORY('Moving spring anchor',
'Moving spring anchor',(#14996));
#14938=PRODUCT_RELATED_PRODUCT_CATEGORY('Upper link','Upper link',(#14997));
#14939=PRODUCT_RELATED_PRODUCT_CATEGORY('200 mm arm (1)',
'200 mm arm (1)',(#14998));
#14940=PRODUCT_RELATED_PRODUCT_CATEGORY('Outer race spacer (2)',
'Outer race spacer (2)',(#14999));
#14941=PRODUCT_RELATED_PRODUCT_CATEGORY('Bearing cap (4)',
'Bearing cap (4)',(#15000));
#14942=PRODUCT_RELATED_PRODUCT_CATEGORY('Bearing cap (5)',
'Bearing cap (5)',(#15001));
#14943=PRODUCT_RELATED_PRODUCT_CATEGORY('Outer race spacer (3)',
'Outer race spacer (3)',(#15002));
#14944=PRODUCT_RELATED_PRODUCT_CATEGORY('Bearing cap (6)',
'Bearing cap (6)',(#15003));
#14945=PRODUCT_RELATED_PRODUCT_CATEGORY('Bearing cap (7)',
'Bearing cap (7)',(#15004));
#14946=PRODUCT_RELATED_PRODUCT_CATEGORY(
'Sealed Ball Bearing - 10 x 30 x 9 mm',
'Sealed Ball Bearing - 10 x 30 x 9 mm',(#15005));
#14947=PRODUCT_RELATED_PRODUCT_CATEGORY('Inner ring','Inner ring',(#15006));
#14948=PRODUCT_RELATED_PRODUCT_CATEGORY('Outer ring','Outer ring',(#15007));
#14949=PRODUCT_RELATED_PRODUCT_CATEGORY('Balls','Balls',(#15008));
#14950=PRODUCT_RELATED_PRODUCT_CATEGORY('Cage','Cage',(#15009));
#14951=PRODUCT_RELATED_PRODUCT_CATEGORY('Seals 2RS','Seals 2RS',(#15010));
#14952=PRODUCT_RELATED_PRODUCT_CATEGORY('M4x10 Cap Screw',
'M4x10 Cap Screw',(#15011));
#14953=PRODUCT_RELATED_PRODUCT_CATEGORY('Level platform link',
'Level platform link',(#15012));
#14954=PRODUCT_RELATED_PRODUCT_CATEGORY('Platform link','Platform link',
(#15013));
#14955=PRODUCT_RELATED_PRODUCT_CATEGORY('Pivot pin (1)','Pivot pin (1)',
(#15014));
#14956=PRODUCT_RELATED_PRODUCT_CATEGORY('Inner race sleeve (2)',
'Inner race sleeve (2)',(#15015));
#14957=PRODUCT_RELATED_PRODUCT_CATEGORY('Rear inner spacer (2)',
'Rear inner spacer (2)',(#15016));
#14958=PRODUCT_RELATED_PRODUCT_CATEGORY('Front spacer (1)',
'Front spacer (1)',(#15017));
#14959=PRODUCT_RELATED_PRODUCT_CATEGORY('Pivot keeper (2)',
'Pivot keeper (2)',(#15018));
#14960=PRODUCT_RELATED_PRODUCT_CATEGORY('Pivot pin (2)','Pivot pin (2)',
(#15019));
#14961=PRODUCT_RELATED_PRODUCT_CATEGORY('Inner race sleeve (3)',
'Inner race sleeve (3)',(#15020));
#14962=PRODUCT_RELATED_PRODUCT_CATEGORY('Rear inner spacer (3)',
'Rear inner spacer (3)',(#15021));
#14963=PRODUCT_RELATED_PRODUCT_CATEGORY('Front spacer (2)',
'Front spacer (2)',(#15022));
#14964=PRODUCT_RELATED_PRODUCT_CATEGORY('Pivot keeper (3)',
'Pivot keeper (3)',(#15023));
#14965=PRODUCT_RELATED_PRODUCT_CATEGORY('Cap Screw - M4x16',
'Cap Screw - M4x16',(#15024));
#14966=APPLICATION_PROTOCOL_DEFINITION('international standard',
'automotive_design',2009,#14967);
#14967=APPLICATION_CONTEXT(
'Core Data for Automotive Mechanical Design Process');
#14968=PRODUCT_CONTEXT('part definition',#14967,'mechanical');
#14969=PRODUCT('PAT-039','PAT-039',
'PAT-039',(#14968));
#14970=PRODUCT('Fixed bracket and counter spring',
'Fixed bracket and counter spring','Fixed bracket and counter spring',(#14968));
#14971=PRODUCT('Base','Base','Base',(#14968));
#14972=PRODUCT('Foot strip','Foot strip','Foot strip',(#14968));
#14973=PRODUCT('Foot strip (1)','Foot strip (1)','Foot strip (1)',(#14968));
#14974=PRODUCT('Fixed link','Fixed link','Fixed link',(#14968));
#14975=PRODUCT('Spring arbor pivot','Spring arbor pivot',
'Spring arbor pivot',(#14968));
#14976=PRODUCT('Inner race sleeve','Inner race sleeve',
'Inner race sleeve',(#14968));
#14977=PRODUCT('Rear inner spacer','Rear inner spacer',
'Rear inner spacer',(#14968));
#14978=PRODUCT('Long front spacer','Long front spacer',
'Long front spacer',(#14968));
#14979=PRODUCT('Pivot keeper','Pivot keeper','Pivot keeper',(#14968));
#14980=PRODUCT('Pivot pin','Pivot pin','Pivot pin',(#14968));
#14981=PRODUCT('Inner race sleeve (1)','Inner race sleeve (1)',
'Inner race sleeve (1)',(#14968));
#14982=PRODUCT('Rear inner spacer (1)','Rear inner spacer (1)',
'Rear inner spacer (1)',(#14968));
#14983=PRODUCT('Front spacer','Front spacer','Front spacer',(#14968));
#14984=PRODUCT('Pivot keeper (1)','Pivot keeper (1)','Pivot keeper (1)',(#14968));
#14985=PRODUCT('Fixed spring bracket','Fixed spring bracket',
'Fixed spring bracket',(#14968));
#14986=PRODUCT('Installed torsion spring','Installed torsion spring',
'Installed torsion spring',(#14968));
#14987=PRODUCT('M5x14 Cap Screw','M5x14 Cap Screw','M5x14 Cap Screw',(#14968));
#14988=PRODUCT('Lower link','Lower link','Lower link',(#14968));
#14989=PRODUCT('200 mm arm','200 mm arm','200 mm arm',(#14968));
#14990=PRODUCT('Outer race spacer','Outer race spacer',
'Outer race spacer',(#14968));
#14991=PRODUCT('Bearing cap','Bearing cap','Bearing cap',(#14968));
#14992=PRODUCT('Bearing cap (1)','Bearing cap (1)','Bearing cap (1)',(#14968));
#14993=PRODUCT('Outer race spacer (1)','Outer race spacer (1)',
'Outer race spacer (1)',(#14968));
#14994=PRODUCT('Bearing cap (2)','Bearing cap (2)','Bearing cap (2)',(#14968));
#14995=PRODUCT('Bearing cap (3)','Bearing cap (3)','Bearing cap (3)',(#14968));
#14996=PRODUCT('Moving spring anchor','Moving spring anchor',
'Moving spring anchor',(#14968));
#14997=PRODUCT('Upper link','Upper link','Upper link',(#14968));
#14998=PRODUCT('200 mm arm (1)','200 mm arm (1)','200 mm arm (1)',(#14968));
#14999=PRODUCT('Outer race spacer (2)','Outer race spacer (2)',
'Outer race spacer (2)',(#14968));
#15000=PRODUCT('Bearing cap (4)','Bearing cap (4)','Bearing cap (4)',(#14968));
#15001=PRODUCT('Bearing cap (5)','Bearing cap (5)','Bearing cap (5)',(#14968));
#15002=PRODUCT('Outer race spacer (3)','Outer race spacer (3)',
'Outer race spacer (3)',(#14968));
#15003=PRODUCT('Bearing cap (6)','Bearing cap (6)','Bearing cap (6)',(#14968));
#15004=PRODUCT('Bearing cap (7)','Bearing cap (7)','Bearing cap (7)',(#14968));
#15005=PRODUCT('Sealed Ball Bearing - 10 x 30 x 9 mm',
'Sealed Ball Bearing - 10 x 30 x 9 mm',
'Sealed Ball Bearing - 10 x 30 x 9 mm',(#14968));
#15006=PRODUCT('Inner ring','Inner ring','Inner ring',(#14968));
#15007=PRODUCT('Outer ring','Outer ring','Outer ring',(#14968));
#15008=PRODUCT('Balls','Balls','Balls',(#14968));
#15009=PRODUCT('Cage','Cage','Cage',(#14968));
#15010=PRODUCT('Seals 2RS','Seals 2RS','Seals 2RS',(#14968));
#15011=PRODUCT('M4x10 Cap Screw','M4x10 Cap Screw','M4x10 Cap Screw',(#14968));
#15012=PRODUCT('Level platform link','Level platform link',
'Level platform link',(#14968));
#15013=PRODUCT('Platform link','Platform link','Platform link',(#14968));
#15014=PRODUCT('Pivot pin (1)','Pivot pin (1)','Pivot pin (1)',(#14968));
#15015=PRODUCT('Inner race sleeve (2)','Inner race sleeve (2)',
'Inner race sleeve (2)',(#14968));
#15016=PRODUCT('Rear inner spacer (2)','Rear inner spacer (2)',
'Rear inner spacer (2)',(#14968));
#15017=PRODUCT('Front spacer (1)','Front spacer (1)','Front spacer (1)',(#14968));
#15018=PRODUCT('Pivot keeper (2)','Pivot keeper (2)','Pivot keeper (2)',(#14968));
#15019=PRODUCT('Pivot pin (2)','Pivot pin (2)','Pivot pin (2)',(#14968));
#15020=PRODUCT('Inner race sleeve (3)','Inner race sleeve (3)',
'Inner race sleeve (3)',(#14968));
#15021=PRODUCT('Rear inner spacer (3)','Rear inner spacer (3)',
'Rear inner spacer (3)',(#14968));
#15022=PRODUCT('Front spacer (2)','Front spacer (2)','Front spacer (2)',(#14968));
#15023=PRODUCT('Pivot keeper (3)','Pivot keeper (3)','Pivot keeper (3)',(#14968));
#15024=PRODUCT('Cap Screw - M4x16','Cap Screw - M4x16',
'Cap Screw - M4x16',(#14968));
#15025=PRESENTATION_STYLE_ASSIGNMENT((#15030));
#15026=PRESENTATION_STYLE_ASSIGNMENT((#15031));
#15027=PRESENTATION_STYLE_ASSIGNMENT((#15032));
#15028=PRESENTATION_STYLE_ASSIGNMENT((#15033));
#15029=PRESENTATION_STYLE_ASSIGNMENT((#15034));
#15030=SURFACE_STYLE_USAGE(.BOTH.,#15035);
#15031=SURFACE_STYLE_USAGE(.BOTH.,#15036);
#15032=SURFACE_STYLE_USAGE(.BOTH.,#15037);
#15033=SURFACE_STYLE_USAGE(.BOTH.,#15038);
#15034=SURFACE_STYLE_USAGE(.BOTH.,#15039);
#15035=SURFACE_SIDE_STYLE('',(#15040));
#15036=SURFACE_SIDE_STYLE('',(#15041));
#15037=SURFACE_SIDE_STYLE('',(#15042));
#15038=SURFACE_SIDE_STYLE('',(#15043));
#15039=SURFACE_SIDE_STYLE('',(#15044));
#15040=SURFACE_STYLE_FILL_AREA(#15045);
#15041=SURFACE_STYLE_FILL_AREA(#15046);
#15042=SURFACE_STYLE_FILL_AREA(#15047);
#15043=SURFACE_STYLE_FILL_AREA(#15048);
#15044=SURFACE_STYLE_FILL_AREA(#15049);
#15045=FILL_AREA_STYLE('Steel - Satin',(#15050));
#15046=FILL_AREA_STYLE('CAD Library Painted - Deep blue',(#15051));
#15047=FILL_AREA_STYLE('CAD Library Painted - Engineering blue',(#15052));
#15048=FILL_AREA_STYLE('CAD Library Painted - Steel gray',(#15053));
#15049=FILL_AREA_STYLE('CAD Library Painted - Graphite',(#15054));
#15050=FILL_AREA_STYLE_COLOUR('Steel - Satin',#15055);
#15051=FILL_AREA_STYLE_COLOUR('CAD Library Painted - Deep blue',#15056);
#15052=FILL_AREA_STYLE_COLOUR('CAD Library Painted - Engineering blue',
#15057);
#15053=FILL_AREA_STYLE_COLOUR('CAD Library Painted - Steel gray',#15058);
#15054=FILL_AREA_STYLE_COLOUR('CAD Library Painted - Graphite',#15059);
#15055=COLOUR_RGB('Steel - Satin',0.627450980392157,0.627450980392157,0.627450980392157);
#15056=COLOUR_RGB('CAD Library Painted - Deep blue',0.0784313725490196,
0.203921568627451,0.349019607843137);
#15057=COLOUR_RGB('CAD Library Painted - Engineering blue',0.12156862745098,
0.356862745098039,0.6);
#15058=COLOUR_RGB('CAD Library Painted - Steel gray',0.592156862745098,
0.631372549019608,0.67843137254902);
#15059=COLOUR_RGB('CAD Library Painted - Graphite',0.168627450980392,0.192156862745098,
0.231372549019608);
#15060=COLOUR_RGB('Dark Blue',0.08,0.2,0.34);
#15061=FILL_AREA_STYLE_COLOUR('',#15060);
#15062=FILL_AREA_STYLE('',(#15061));
#15063=SURFACE_STYLE_FILL_AREA(#15062);
#15064=SURFACE_SIDE_STYLE('',(#15063));
#15065=SURFACE_STYLE_USAGE(.BOTH.,#15064);
#15066=PRESENTATION_STYLE_ASSIGNMENT((#15065));
#15067=COLOUR_RGB('Light Blue',0.38,0.62,0.78);
#15068=FILL_AREA_STYLE_COLOUR('',#15067);
#15069=FILL_AREA_STYLE('',(#15068));
#15070=SURFACE_STYLE_FILL_AREA(#15069);
#15071=SURFACE_SIDE_STYLE('',(#15070));
#15072=SURFACE_STYLE_USAGE(.BOTH.,#15071);
#15073=PRESENTATION_STYLE_ASSIGNMENT((#15072));
#15074=COLOUR_RGB('Sky Blue',0.24,0.69,0.87);
#15075=FILL_AREA_STYLE_COLOUR('',#15074);
#15076=FILL_AREA_STYLE('',(#15075));
#15077=SURFACE_STYLE_FILL_AREA(#15076);
#15078=SURFACE_SIDE_STYLE('',(#15077));
#15079=SURFACE_STYLE_USAGE(.BOTH.,#15078);
#15080=PRESENTATION_STYLE_ASSIGNMENT((#15079));
#15081=COLOUR_RGB('Grey',0.48,0.52,0.57);
#15082=FILL_AREA_STYLE_COLOUR('',#15081);
#15083=FILL_AREA_STYLE('',(#15082));
#15084=SURFACE_STYLE_FILL_AREA(#15083);
#15085=SURFACE_SIDE_STYLE('',(#15084));
#15086=SURFACE_STYLE_USAGE(.BOTH.,#15085);
#15087=PRESENTATION_STYLE_ASSIGNMENT((#15086));
#15088=COLOUR_RGB('Black',0.12,0.14,0.17);
#15089=FILL_AREA_STYLE_COLOUR('',#15088);
#15090=FILL_AREA_STYLE('',(#15089));
#15091=SURFACE_STYLE_FILL_AREA(#15090);
#15092=SURFACE_SIDE_STYLE('',(#15091));
#15093=SURFACE_STYLE_USAGE(.BOTH.,#15092);
#15094=PRESENTATION_STYLE_ASSIGNMENT((#15093));
#15095=COLOUR_RGB('Off White',0.89,0.88,0.83);
#15096=FILL_AREA_STYLE_COLOUR('',#15095);
#15097=FILL_AREA_STYLE('',(#15096));
#15098=SURFACE_STYLE_FILL_AREA(#15097);
#15099=SURFACE_SIDE_STYLE('',(#15098));
#15100=SURFACE_STYLE_USAGE(.BOTH.,#15099);
#15101=PRESENTATION_STYLE_ASSIGNMENT((#15100));
ENDSEC;
END-ISO-10303-21;
